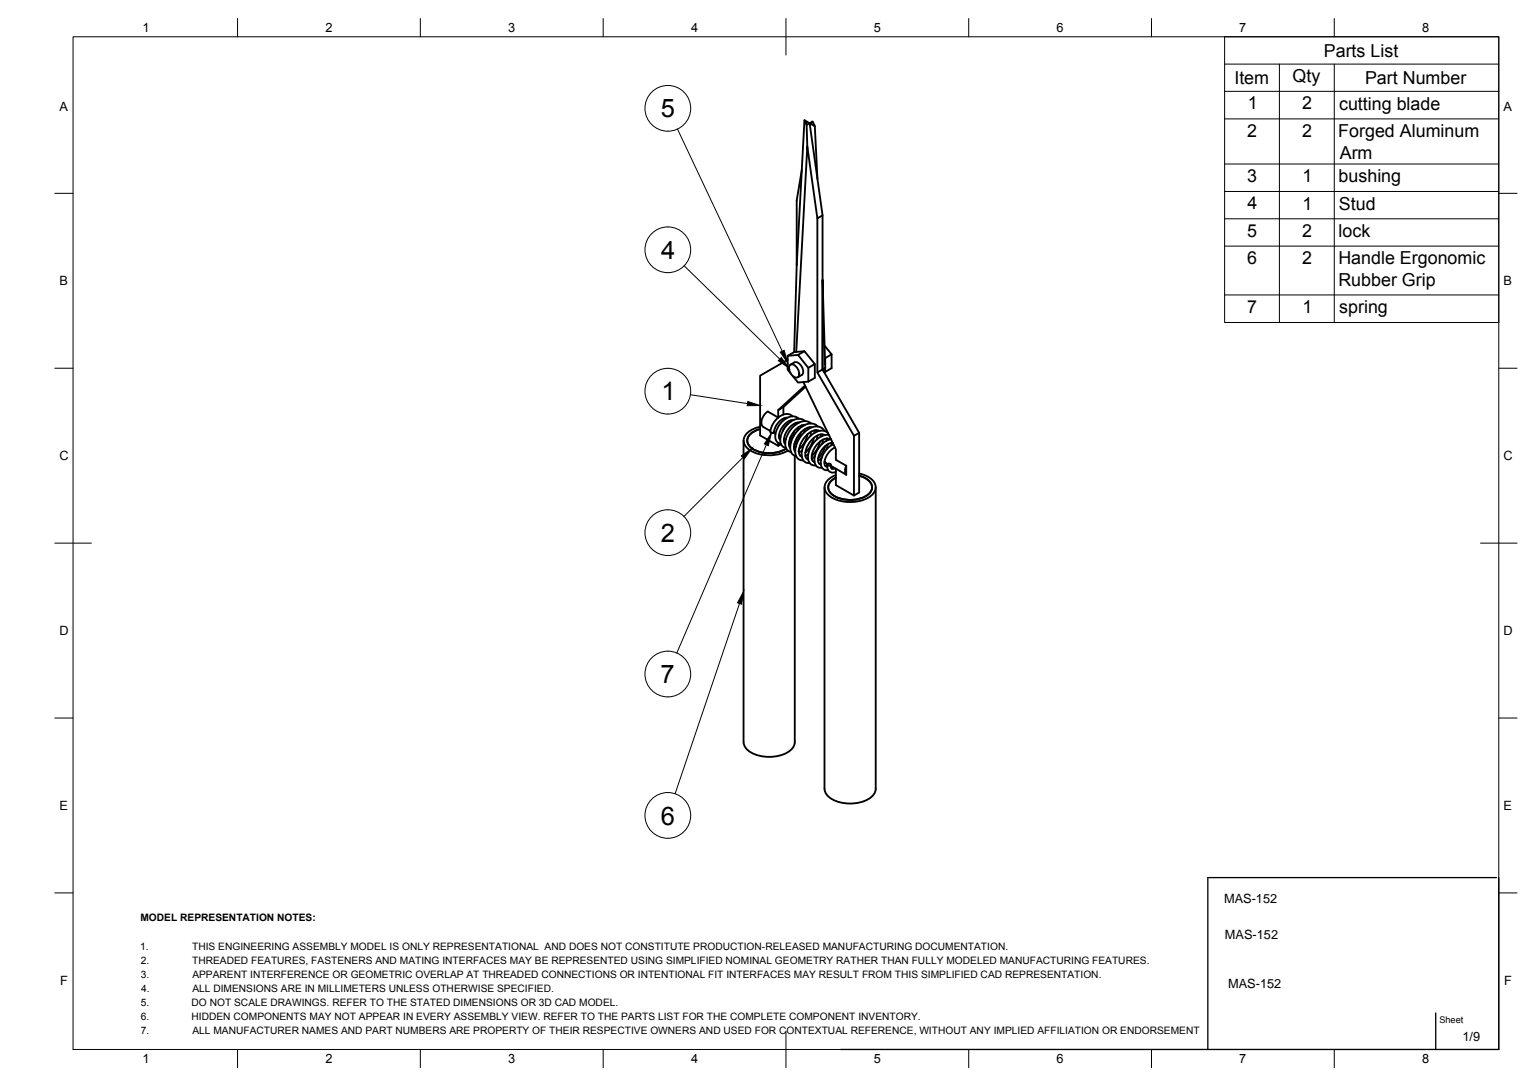
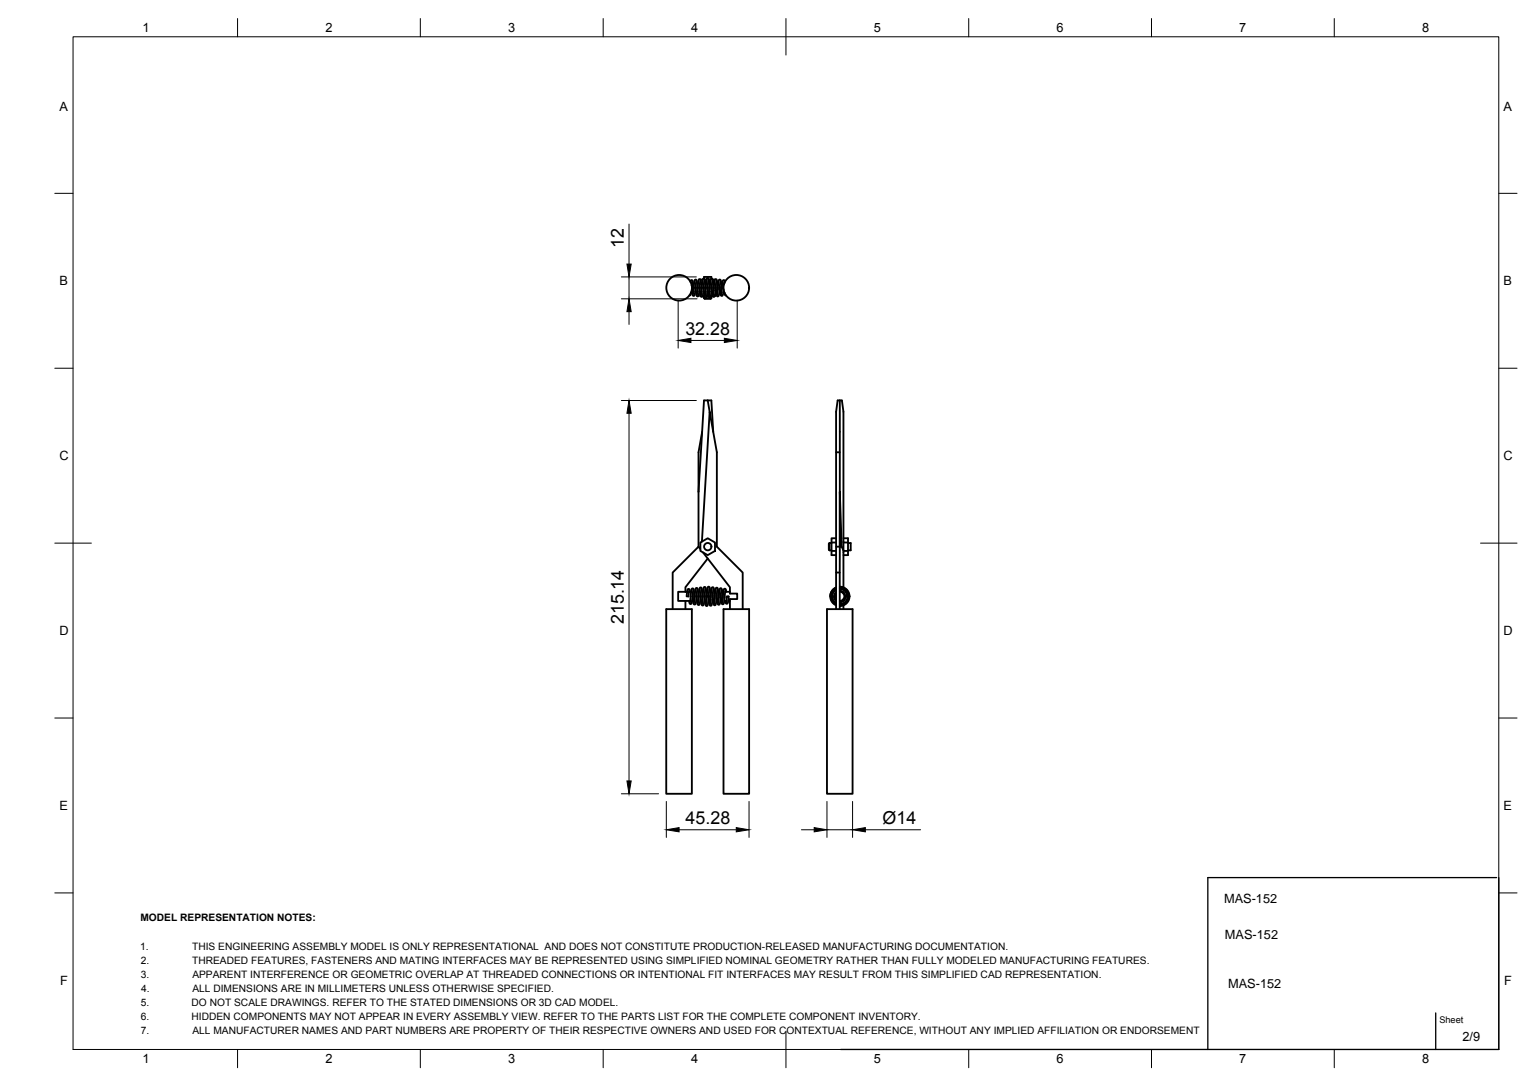
ISO-10303-21;
HEADER;
/* Generated by software containing ST-Developer
 * from STEP Tools, Inc. (www.steptools.com) 
 */

FILE_DESCRIPTION(
/* description */ ('STEP AP214'),
/* implementation_level */ '2;1');

FILE_NAME(
/* name */ 'MAS-152',
/* time_stamp */ '2026-11-04T19:18:53-08:00',
/* author */ (''),
/* organization */ (''),
/* preprocessor_version */ 'ST-DEVELOPER v20.2',
/* originating_system */ 'Autodesk Translation Framework v15.17.0.0',
/* authorisation */ '');

FILE_SCHEMA (('AUTOMOTIVE_DESIGN { 1 0 10303 214 3 1 1 }'));
ENDSEC;

DATA;
#10=MECHANICAL_DESIGN_GEOMETRIC_PRESENTATION_REPRESENTATION('',(#78,#79,
#80,#81,#82,#83,#84),#5942);
#11=ITEM_DEFINED_TRANSFORMATION($,$,#1040,#1100);
#12=ITEM_DEFINED_TRANSFORMATION($,$,#1067,#1101);
#13=ITEM_DEFINED_TRANSFORMATION($,$,#1011,#1102);
#14=ITEM_DEFINED_TRANSFORMATION($,$,#1020,#1103);
#15=ITEM_DEFINED_TRANSFORMATION($,$,#1088,#1104);
#16=ITEM_DEFINED_TRANSFORMATION($,$,#1078,#1105);
#17=ITEM_DEFINED_TRANSFORMATION($,$,#1029,#1106);
#18=ITEM_DEFINED_TRANSFORMATION($,$,#1040,#1107);
#19=ITEM_DEFINED_TRANSFORMATION($,$,#1067,#1108);
#20=ITEM_DEFINED_TRANSFORMATION($,$,#1078,#1109);
#21=ITEM_DEFINED_TRANSFORMATION($,$,#1088,#1110);
#22=(
REPRESENTATION_RELATIONSHIP($,$,#5978,#5974)
REPRESENTATION_RELATIONSHIP_WITH_TRANSFORMATION(#11)
SHAPE_REPRESENTATION_RELATIONSHIP()
);
#23=(
REPRESENTATION_RELATIONSHIP($,$,#5979,#5974)
REPRESENTATION_RELATIONSHIP_WITH_TRANSFORMATION(#12)
SHAPE_REPRESENTATION_RELATIONSHIP()
);
#24=(
REPRESENTATION_RELATIONSHIP($,$,#5975,#5974)
REPRESENTATION_RELATIONSHIP_WITH_TRANSFORMATION(#13)
SHAPE_REPRESENTATION_RELATIONSHIP()
);
#25=(
REPRESENTATION_RELATIONSHIP($,$,#5976,#5974)
REPRESENTATION_RELATIONSHIP_WITH_TRANSFORMATION(#14)
SHAPE_REPRESENTATION_RELATIONSHIP()
);
#26=(
REPRESENTATION_RELATIONSHIP($,$,#5981,#5974)
REPRESENTATION_RELATIONSHIP_WITH_TRANSFORMATION(#15)
SHAPE_REPRESENTATION_RELATIONSHIP()
);
#27=(
REPRESENTATION_RELATIONSHIP($,$,#5980,#5974)
REPRESENTATION_RELATIONSHIP_WITH_TRANSFORMATION(#16)
SHAPE_REPRESENTATION_RELATIONSHIP()
);
#28=(
REPRESENTATION_RELATIONSHIP($,$,#5977,#5974)
REPRESENTATION_RELATIONSHIP_WITH_TRANSFORMATION(#17)
SHAPE_REPRESENTATION_RELATIONSHIP()
);
#29=(
REPRESENTATION_RELATIONSHIP($,$,#5978,#5974)
REPRESENTATION_RELATIONSHIP_WITH_TRANSFORMATION(#18)
SHAPE_REPRESENTATION_RELATIONSHIP()
);
#30=(
REPRESENTATION_RELATIONSHIP($,$,#5979,#5974)
REPRESENTATION_RELATIONSHIP_WITH_TRANSFORMATION(#19)
SHAPE_REPRESENTATION_RELATIONSHIP()
);
#31=(
REPRESENTATION_RELATIONSHIP($,$,#5980,#5974)
REPRESENTATION_RELATIONSHIP_WITH_TRANSFORMATION(#20)
SHAPE_REPRESENTATION_RELATIONSHIP()
);
#32=(
REPRESENTATION_RELATIONSHIP($,$,#5981,#5974)
REPRESENTATION_RELATIONSHIP_WITH_TRANSFORMATION(#21)
SHAPE_REPRESENTATION_RELATIONSHIP()
);
#33=CONTEXT_DEPENDENT_SHAPE_REPRESENTATION(#22,#5963);
#34=CONTEXT_DEPENDENT_SHAPE_REPRESENTATION(#23,#5964);
#35=CONTEXT_DEPENDENT_SHAPE_REPRESENTATION(#24,#5965);
#36=CONTEXT_DEPENDENT_SHAPE_REPRESENTATION(#25,#5966);
#37=CONTEXT_DEPENDENT_SHAPE_REPRESENTATION(#26,#5967);
#38=CONTEXT_DEPENDENT_SHAPE_REPRESENTATION(#27,#5968);
#39=CONTEXT_DEPENDENT_SHAPE_REPRESENTATION(#28,#5969);
#40=CONTEXT_DEPENDENT_SHAPE_REPRESENTATION(#29,#5970);
#41=CONTEXT_DEPENDENT_SHAPE_REPRESENTATION(#30,#5971);
#42=CONTEXT_DEPENDENT_SHAPE_REPRESENTATION(#31,#5972);
#43=CONTEXT_DEPENDENT_SHAPE_REPRESENTATION(#32,#5973);
#44=NEXT_ASSEMBLY_USAGE_OCCURRENCE('Cutting Blade:1','Cutting Blade:1',
'Cutting Blade:1',#5983,#5987,'Cutting Blade:1');
#45=NEXT_ASSEMBLY_USAGE_OCCURRENCE('Forged Aluminum Arm:1',
'Forged Aluminum Arm:1','Forged Aluminum Arm:1',#5983,#5988,
'Forged Aluminum Arm:1');
#46=NEXT_ASSEMBLY_USAGE_OCCURRENCE('bushing:1','bushing:1','bushing:1',
#5983,#5984,'bushing:1');
#47=NEXT_ASSEMBLY_USAGE_OCCURRENCE('stud:1','stud:1','stud:1',#5983,#5985,
'stud:1');
#48=NEXT_ASSEMBLY_USAGE_OCCURRENCE('lock:1','lock:1','lock:1',#5983,#5990,
'lock:1');
#49=NEXT_ASSEMBLY_USAGE_OCCURRENCE('Handle Ergonomic Rubber Grip:1',
'Handle Ergonomic Rubber Grip:1','Handle Ergonomic Rubber Grip:1',#5983,
#5989,'Handle Ergonomic Rubber Grip:1');
#50=NEXT_ASSEMBLY_USAGE_OCCURRENCE('spring:1','spring:1','spring:1',#5983,
#5986,'spring:1');
#51=NEXT_ASSEMBLY_USAGE_OCCURRENCE('Cutting Blade:2','Cutting Blade:2',
'Cutting Blade:2',#5983,#5987,'Cutting Blade:2');
#52=NEXT_ASSEMBLY_USAGE_OCCURRENCE('Forged Aluminum Arm:2',
'Forged Aluminum Arm:2','Forged Aluminum Arm:2',#5983,#5988,
'Forged Aluminum Arm:2');
#53=NEXT_ASSEMBLY_USAGE_OCCURRENCE('Handle Ergonomic Rubber Grip:2',
'Handle Ergonomic Rubber Grip:2','Handle Ergonomic Rubber Grip:2',#5983,
#5989,'Handle Ergonomic Rubber Grip:2');
#54=NEXT_ASSEMBLY_USAGE_OCCURRENCE('lock:2','lock:2','lock:2',#5983,#5990,
'lock:2');
#55=B_SPLINE_CURVE_WITH_KNOTS('',3,(#2155,#2156,#2157,#2158,#2159,#2160,
#2161,#2162,#2163,#2164,#2165,#2166,#2167,#2168,#2169,#2170,#2171,#2172,
#2173,#2174,#2175,#2176,#2177,#2178,#2179,#2180,#2181,#2182,#2183,#2184,
#2185,#2186,#2187,#2188,#2189,#2190,#2191,#2192,#2193,#2194,#2195,#2196,
#2197,#2198,#2199,#2200,#2201,#2202,#2203,#2204,#2205,#2206,#2207,#2208,
#2209,#2210,#2211,#2212,#2213,#2214,#2215,#2216,#2217,#2218,#2219,#2220,
#2221,#2222,#2223,#2224,#2225,#2226,#2227,#2228,#2229,#2230,#2231,#2232,
#2233,#2234,#2235,#2236,#2237,#2238,#2239,#2240,#2241,#2242,#2243,#2244,
#2245,#2246,#2247,#2248,#2249,#2250,#2251,#2252,#2253,#2254,#2255,#2256,
#2257,#2258,#2259,#2260,#2261,#2262,#2263,#2264,#2265,#2266,#2267,#2268,
#2269,#2270,#2271,#2272,#2273,#2274,#2275,#2276,#2277,#2278,#2279,#2280,
#2281,#2282,#2283,#2284,#2285,#2286,#2287,#2288,#2289,#2290,#2291,#2292,
#2293,#2294,#2295,#2296,#2297,#2298,#2299,#2300,#2301,#2302,#2303,#2304,
#2305,#2306,#2307,#2308),.UNSPECIFIED.,.F.,.F.,(4,3,3,3,3,3,3,3,3,3,3,3,
3,3,3,3,3,3,3,3,3,3,3,3,3,3,3,3,3,3,3,3,3,3,3,3,3,3,3,3,3,3,3,3,3,3,3,3,
3,3,3,4),(8.16441129645516E-18,0.0155213821795324,0.0465641465385971,0.0776069108976618,
0.108649675256726,0.139692439615791,0.170735203974856,0.201777968333921,
0.232820732692985,0.26386349705205,0.294906261411162,0.325949025770274,
0.356991790129291,0.388034554488308,0.419077318847373,0.450120083206437,
0.46564146538597,0.481162847565502,0.496684229745034,0.512205611924566,
0.527726994104099,0.543248376283631,0.558769758463163,0.574291140642696,
0.589812522822228,0.605333905001761,0.620855287181293,0.636376669360825,
0.651898051540357,0.66741943371989,0.682940815899422,0.698462198078954,
0.713983580258487,0.729504962438019,0.745026344617551,0.760547726797084,
0.776069108976616,0.791590491156148,0.807111873335681,0.822633255515213,
0.838154637694745,0.853676019874278,0.86919740205381,0.884718784233342,
0.900240166412875,0.915761548592407,0.931282930771939,0.946804312951471,
0.973402156475736,0.986701078237868,0.993350539118934,0.993460673612188),
 .UNSPECIFIED.);
#56=B_SPLINE_CURVE_WITH_KNOTS('',3,(#2313,#2314,#2315,#2316,#2317,#2318,
#2319,#2320,#2321,#2322,#2323,#2324,#2325,#2326,#2327,#2328,#2329,#2330,
#2331,#2332,#2333,#2334,#2335,#2336,#2337,#2338,#2339,#2340,#2341,#2342,
#2343,#2344,#2345,#2346,#2347,#2348,#2349,#2350,#2351,#2352,#2353,#2354,
#2355,#2356,#2357,#2358,#2359,#2360,#2361,#2362,#2363,#2364,#2365,#2366,
#2367,#2368,#2369,#2370,#2371,#2372,#2373,#2374,#2375,#2376,#2377,#2378,
#2379,#2380,#2381,#2382,#2383,#2384,#2385,#2386,#2387,#2388,#2389,#2390,
#2391,#2392,#2393,#2394,#2395,#2396,#2397,#2398,#2399,#2400,#2401,#2402,
#2403,#2404,#2405,#2406,#2407,#2408,#2409,#2410,#2411,#2412,#2413,#2414,
#2415,#2416,#2417,#2418,#2419,#2420,#2421,#2422,#2423,#2424,#2425,#2426,
#2427,#2428,#2429,#2430,#2431,#2432,#2433,#2434,#2435,#2436,#2437,#2438,
#2439,#2440,#2441,#2442,#2443,#2444,#2445,#2446,#2447,#2448,#2449,#2450,
#2451,#2452,#2453,#2454,#2455,#2456,#2457,#2458,#2459,#2460,#2461,#2462,
#2463),.UNSPECIFIED.,.F.,.F.,(4,3,3,3,3,3,3,3,3,3,3,3,3,3,3,3,3,3,3,3,3,
3,3,3,3,3,3,3,3,3,3,3,3,3,3,3,3,3,3,3,3,3,3,3,3,3,3,3,3,3,4),(0.,0.0155213821795324,
0.0465641465385971,0.0776069108976618,0.108649675256726,0.139692439615791,
0.170735203974856,0.201777968333921,0.232820732692985,0.26386349705205,
0.294906261411162,0.325949025770274,0.356991790129291,0.388034554488308,
0.419077318847373,0.450120083206437,0.46564146538597,0.481162847565502,
0.496684229745034,0.512205611924566,0.527726994104099,0.543248376283631,
0.558769758463163,0.574291140642696,0.589812522822228,0.605333905001761,
0.620855287181293,0.636376669360825,0.651898051540357,0.66741943371989,
0.682940815899422,0.698462198078954,0.713983580258487,0.729504962438019,
0.745026344617551,0.760547726797084,0.776069108976616,0.791590491156148,
0.807111873335681,0.822633255515213,0.838154637694745,0.853676019874278,
0.86919740205381,0.884718784233342,0.900240166412875,0.915761548592407,
0.931282930771939,0.946804312951471,0.973402156475736,0.986701078237868,
0.993275477626297),.UNSPECIFIED.);
#57=B_SPLINE_CURVE_WITH_KNOTS('',3,(#3378,#3379,#3380,#3381,#3382,#3383,
#3384,#3385,#3386,#3387,#3388,#3389,#3390,#3391,#3392,#3393,#3394,#3395,
#3396,#3397,#3398,#3399,#3400,#3401,#3402,#3403,#3404,#3405,#3406,#3407,
#3408,#3409,#3410,#3411,#3412,#3413,#3414,#3415,#3416,#3417,#3418,#3419,
#3420,#3421,#3422,#3423,#3424,#3425,#3426,#3427,#3428,#3429,#3430,#3431,
#3432,#3433,#3434,#3435,#3436,#3437,#3438,#3439,#3440,#3441,#3442,#3443,
#3444,#3445,#3446,#3447,#3448,#3449,#3450,#3451,#3452,#3453,#3454,#3455,
#3456,#3457,#3458,#3459,#3460,#3461,#3462,#3463,#3464,#3465,#3466,#3467,
#3468,#3469,#3470,#3471,#3472,#3473,#3474,#3475,#3476,#3477,#3478,#3479,
#3480,#3481,#3482,#3483,#3484,#3485,#3486,#3487,#3488,#3489,#3490,#3491,
#3492,#3493,#3494,#3495,#3496,#3497,#3498,#3499,#3500,#3501,#3502,#3503,
#3504,#3505,#3506,#3507,#3508,#3509,#3510,#3511,#3512,#3513,#3514,#3515,
#3516,#3517,#3518,#3519,#3520,#3521,#3522,#3523,#3524,#3525,#3526,#3527,
#3528,#3529,#3530,#3531,#3532,#3533,#3534,#3535,#3536,#3537,#3538,#3539,
#3540,#3541,#3542,#3543,#3544,#3545,#3546,#3547,#3548,#3549,#3550,#3551,
#3552,#3553,#3554,#3555,#3556,#3557,#3558,#3559,#3560,#3561,#3562,#3563,
#3564,#3565,#3566,#3567,#3568,#3569,#3570),.UNSPECIFIED.,.F.,.F.,(4,3,3,
3,3,3,3,3,3,3,3,3,3,3,3,3,3,3,3,3,3,3,3,3,3,3,3,3,3,3,3,3,3,3,3,3,3,3,3,
3,3,3,3,3,3,3,3,3,3,3,3,3,3,3,3,3,3,3,3,3,3,3,3,3,4),(-3.92493609792139E-18,
0.015625,0.03125,0.046875,0.0625,0.078125,0.09375,0.109375,0.125,0.140625,
0.15625,0.171875,0.1875,0.203125,0.21875,0.234375,0.25,0.265625,0.28125,
0.296875,0.3125,0.328125,0.34375,0.359375,0.375,0.390625,0.40625,0.421875,
0.4375,0.453125,0.46875,0.484375,0.5,0.515625,0.53125,0.546875,0.5625,0.578125,
0.59375,0.609375,0.625,0.640625,0.65625,0.671875,0.6875,0.703125,0.71875,
0.734375,0.75,0.765625,0.78125,0.796875,0.8125,0.828125,0.84375,0.859375,
0.875,0.890625,0.90625,0.921875,0.9375,0.953125,0.96875,0.984375,1.),
 .UNSPECIFIED.);
#58=B_SPLINE_CURVE_WITH_KNOTS('',3,(#3572,#3573,#3574,#3575,#3576,#3577,
#3578,#3579,#3580,#3581,#3582,#3583,#3584,#3585,#3586,#3587,#3588,#3589,
#3590,#3591,#3592,#3593,#3594,#3595,#3596,#3597,#3598,#3599,#3600,#3601,
#3602,#3603,#3604,#3605,#3606,#3607,#3608,#3609,#3610,#3611,#3612,#3613,
#3614,#3615,#3616,#3617,#3618,#3619,#3620,#3621,#3622,#3623,#3624,#3625,
#3626,#3627,#3628,#3629,#3630,#3631,#3632,#3633,#3634,#3635,#3636,#3637,
#3638,#3639,#3640,#3641,#3642,#3643,#3644,#3645,#3646,#3647,#3648,#3649,
#3650,#3651,#3652,#3653,#3654,#3655,#3656,#3657,#3658,#3659,#3660,#3661,
#3662,#3663,#3664,#3665,#3666,#3667,#3668,#3669,#3670,#3671,#3672,#3673,
#3674,#3675,#3676,#3677,#3678,#3679,#3680,#3681,#3682,#3683,#3684,#3685,
#3686,#3687,#3688,#3689,#3690,#3691,#3692,#3693,#3694,#3695,#3696,#3697,
#3698,#3699,#3700,#3701,#3702,#3703,#3704,#3705,#3706,#3707,#3708,#3709,
#3710,#3711,#3712,#3713,#3714,#3715,#3716,#3717,#3718,#3719,#3720,#3721,
#3722,#3723,#3724,#3725,#3726,#3727,#3728,#3729,#3730,#3731,#3732,#3733,
#3734,#3735,#3736,#3737,#3738,#3739,#3740,#3741,#3742,#3743,#3744,#3745,
#3746,#3747,#3748,#3749,#3750,#3751,#3752,#3753,#3754,#3755,#3756,#3757,
#3758,#3759,#3760,#3761,#3762,#3763,#3764),.UNSPECIFIED.,.F.,.F.,(4,3,3,
3,3,3,3,3,3,3,3,3,3,3,3,3,3,3,3,3,3,3,3,3,3,3,3,3,3,3,3,3,3,3,3,3,3,3,3,
3,3,3,3,3,3,3,3,3,3,3,3,3,3,3,3,3,3,3,3,3,3,3,3,3,4),(0.,0.015625,0.03125,
0.046875,0.0625,0.078125,0.09375,0.109375,0.125,0.140625,0.15625,0.171875,
0.1875,0.203125,0.21875,0.234375,0.25,0.265625,0.28125,0.296875,0.3125,
0.328125,0.34375,0.359375,0.375,0.390625,0.40625,0.421875,0.4375,0.453125,
0.46875,0.484375,0.5,0.515625,0.53125,0.546875,0.5625,0.578125,0.59375,
0.609375,0.625,0.640625,0.65625,0.671875,0.6875,0.703125,0.71875,0.734375,
0.75,0.765625,0.78125,0.796875,0.8125,0.828125,0.84375,0.859375,0.875,0.890625,
0.90625,0.921875,0.9375,0.953125,0.96875,0.984375,1.),.UNSPECIFIED.);
#59=(
BOUNDED_SURFACE()
B_SPLINE_SURFACE(3,3,((#1423,#1424,#1425,#1426,#1427,#1428,#1429,#1430,
#1431,#1432,#1433,#1434,#1435,#1436,#1437,#1438,#1439,#1440,#1441,#1442,
#1443,#1444,#1445,#1446,#1447,#1448,#1449,#1450,#1451,#1452,#1453,#1454,
#1455,#1456,#1457,#1458,#1459,#1460,#1461,#1462,#1463,#1464,#1465,#1466,
#1467,#1468,#1469,#1470,#1471,#1472,#1473,#1474,#1475,#1476,#1477,#1478,
#1479,#1480,#1481,#1482,#1483,#1484,#1485,#1486,#1487,#1488,#1489,#1490,
#1491,#1492,#1493,#1494,#1495,#1496,#1497,#1498,#1499,#1500,#1501,#1502,
#1503,#1504,#1505,#1506,#1507,#1508,#1509,#1510,#1511,#1512,#1513,#1514,
#1515,#1516,#1517,#1518,#1519,#1520,#1521,#1522,#1523,#1524,#1525,#1526),
(#1527,#1528,#1529,#1530,#1531,#1532,#1533,#1534,#1535,#1536,#1537,#1538,
#1539,#1540,#1541,#1542,#1543,#1544,#1545,#1546,#1547,#1548,#1549,#1550,
#1551,#1552,#1553,#1554,#1555,#1556,#1557,#1558,#1559,#1560,#1561,#1562,
#1563,#1564,#1565,#1566,#1567,#1568,#1569,#1570,#1571,#1572,#1573,#1574,
#1575,#1576,#1577,#1578,#1579,#1580,#1581,#1582,#1583,#1584,#1585,#1586,
#1587,#1588,#1589,#1590,#1591,#1592,#1593,#1594,#1595,#1596,#1597,#1598,
#1599,#1600,#1601,#1602,#1603,#1604,#1605,#1606,#1607,#1608,#1609,#1610,
#1611,#1612,#1613,#1614,#1615,#1616,#1617,#1618,#1619,#1620,#1621,#1622,
#1623,#1624,#1625,#1626,#1627,#1628,#1629,#1630),(#1631,#1632,#1633,#1634,
#1635,#1636,#1637,#1638,#1639,#1640,#1641,#1642,#1643,#1644,#1645,#1646,
#1647,#1648,#1649,#1650,#1651,#1652,#1653,#1654,#1655,#1656,#1657,#1658,
#1659,#1660,#1661,#1662,#1663,#1664,#1665,#1666,#1667,#1668,#1669,#1670,
#1671,#1672,#1673,#1674,#1675,#1676,#1677,#1678,#1679,#1680,#1681,#1682,
#1683,#1684,#1685,#1686,#1687,#1688,#1689,#1690,#1691,#1692,#1693,#1694,
#1695,#1696,#1697,#1698,#1699,#1700,#1701,#1702,#1703,#1704,#1705,#1706,
#1707,#1708,#1709,#1710,#1711,#1712,#1713,#1714,#1715,#1716,#1717,#1718,
#1719,#1720,#1721,#1722,#1723,#1724,#1725,#1726,#1727,#1728,#1729,#1730,
#1731,#1732,#1733,#1734),(#1735,#1736,#1737,#1738,#1739,#1740,#1741,#1742,
#1743,#1744,#1745,#1746,#1747,#1748,#1749,#1750,#1751,#1752,#1753,#1754,
#1755,#1756,#1757,#1758,#1759,#1760,#1761,#1762,#1763,#1764,#1765,#1766,
#1767,#1768,#1769,#1770,#1771,#1772,#1773,#1774,#1775,#1776,#1777,#1778,
#1779,#1780,#1781,#1782,#1783,#1784,#1785,#1786,#1787,#1788,#1789,#1790,
#1791,#1792,#1793,#1794,#1795,#1796,#1797,#1798,#1799,#1800,#1801,#1802,
#1803,#1804,#1805,#1806,#1807,#1808,#1809,#1810,#1811,#1812,#1813,#1814,
#1815,#1816,#1817,#1818,#1819,#1820,#1821,#1822,#1823,#1824,#1825,#1826,
#1827,#1828,#1829,#1830,#1831,#1832,#1833,#1834,#1835,#1836,#1837,#1838),
(#1839,#1840,#1841,#1842,#1843,#1844,#1845,#1846,#1847,#1848,#1849,#1850,
#1851,#1852,#1853,#1854,#1855,#1856,#1857,#1858,#1859,#1860,#1861,#1862,
#1863,#1864,#1865,#1866,#1867,#1868,#1869,#1870,#1871,#1872,#1873,#1874,
#1875,#1876,#1877,#1878,#1879,#1880,#1881,#1882,#1883,#1884,#1885,#1886,
#1887,#1888,#1889,#1890,#1891,#1892,#1893,#1894,#1895,#1896,#1897,#1898,
#1899,#1900,#1901,#1902,#1903,#1904,#1905,#1906,#1907,#1908,#1909,#1910,
#1911,#1912,#1913,#1914,#1915,#1916,#1917,#1918,#1919,#1920,#1921,#1922,
#1923,#1924,#1925,#1926,#1927,#1928,#1929,#1930,#1931,#1932,#1933,#1934,
#1935,#1936,#1937,#1938,#1939,#1940,#1941,#1942),(#1943,#1944,#1945,#1946,
#1947,#1948,#1949,#1950,#1951,#1952,#1953,#1954,#1955,#1956,#1957,#1958,
#1959,#1960,#1961,#1962,#1963,#1964,#1965,#1966,#1967,#1968,#1969,#1970,
#1971,#1972,#1973,#1974,#1975,#1976,#1977,#1978,#1979,#1980,#1981,#1982,
#1983,#1984,#1985,#1986,#1987,#1988,#1989,#1990,#1991,#1992,#1993,#1994,
#1995,#1996,#1997,#1998,#1999,#2000,#2001,#2002,#2003,#2004,#2005,#2006,
#2007,#2008,#2009,#2010,#2011,#2012,#2013,#2014,#2015,#2016,#2017,#2018,
#2019,#2020,#2021,#2022,#2023,#2024,#2025,#2026,#2027,#2028,#2029,#2030,
#2031,#2032,#2033,#2034,#2035,#2036,#2037,#2038,#2039,#2040,#2041,#2042,
#2043,#2044,#2045,#2046),(#2047,#2048,#2049,#2050,#2051,#2052,#2053,#2054,
#2055,#2056,#2057,#2058,#2059,#2060,#2061,#2062,#2063,#2064,#2065,#2066,
#2067,#2068,#2069,#2070,#2071,#2072,#2073,#2074,#2075,#2076,#2077,#2078,
#2079,#2080,#2081,#2082,#2083,#2084,#2085,#2086,#2087,#2088,#2089,#2090,
#2091,#2092,#2093,#2094,#2095,#2096,#2097,#2098,#2099,#2100,#2101,#2102,
#2103,#2104,#2105,#2106,#2107,#2108,#2109,#2110,#2111,#2112,#2113,#2114,
#2115,#2116,#2117,#2118,#2119,#2120,#2121,#2122,#2123,#2124,#2125,#2126,
#2127,#2128,#2129,#2130,#2131,#2132,#2133,#2134,#2135,#2136,#2137,#2138,
#2139,#2140,#2141,#2142,#2143,#2144,#2145,#2146,#2147,#2148,#2149,#2150)),
 .UNSPECIFIED.,.T.,.F.,.F.)
B_SPLINE_SURFACE_WITH_KNOTS((4,3,4),(4,2,2,2,2,2,2,2,2,2,2,2,2,2,2,2,2,
2,2,2,2,2,2,2,2,2,2,2,2,2,2,2,2,2,2,2,2,2,2,2,2,2,2,2,2,2,2,2,2,2,2,4),
(0.,0.5,1.),(0.,0.0155213821795324,0.0465641465385971,0.0776069108976618,
0.108649675256726,0.139692439615791,0.170735203974856,0.201777968333921,
0.232820732692985,0.26386349705205,0.294906261411162,0.325949025770274,
0.356991790129291,0.388034554488308,0.419077318847373,0.450120083206437,
0.46564146538597,0.481162847565502,0.496684229745034,0.512205611924566,
0.527726994104099,0.543248376283631,0.558769758463163,0.574291140642696,
0.589812522822228,0.605333905001761,0.620855287181293,0.636376669360825,
0.651898051540357,0.66741943371989,0.682940815899422,0.698462198078954,
0.713983580258487,0.729504962438019,0.745026344617551,0.760547726797084,
0.776069108976616,0.791590491156148,0.807111873335681,0.822633255515213,
0.838154637694745,0.853676019874278,0.86919740205381,0.884718784233342,
0.900240166412875,0.915761548592407,0.931282930771939,0.946804312951471,
0.973402156475736,0.986701078237868,0.993350539118934,1.),.UNSPECIFIED.)
GEOMETRIC_REPRESENTATION_ITEM()
RATIONAL_B_SPLINE_SURFACE(((1.,1.,1.,1.,1.,1.,1.,1.,1.,1.,1.,1.,1.,1.,1.,
1.,1.,1.,1.,1.,1.,1.,1.,1.,1.,1.,1.,1.,1.,1.,1.,1.,1.,1.,1.,1.,1.,1.,1.,
1.,1.,1.,1.,1.,1.,1.,1.,1.,1.,1.,1.,1.,1.,1.,1.,1.,1.,1.,1.,1.,1.,1.,1.,
1.,1.,1.,1.,1.,1.,1.,1.,1.,1.,1.,1.,1.,1.,1.,1.,1.,1.,1.,1.,1.,1.,1.,1.,
1.,1.,1.,1.,1.,1.,1.,1.,1.,1.,1.,1.,1.,1.,1.,1.,1.),(0.333333333333333,
0.333333333333333,0.333333333333333,0.333333333333333,0.333333333333333,
0.333333333333333,0.333333333333333,0.333333333333333,0.333333333333333,
0.333333333333333,0.333333333333333,0.333333333333333,0.333333333333333,
0.333333333333333,0.333333333333333,0.333333333333333,0.333333333333333,
0.333333333333333,0.333333333333333,0.333333333333333,0.333333333333333,
0.333333333333333,0.333333333333333,0.333333333333333,0.333333333333333,
0.333333333333333,0.333333333333333,0.333333333333333,0.333333333333333,
0.333333333333333,0.333333333333333,0.333333333333333,0.333333333333333,
0.333333333333333,0.333333333333333,0.333333333333333,0.333333333333333,
0.333333333333333,0.333333333333333,0.333333333333333,0.333333333333333,
0.333333333333333,0.333333333333333,0.333333333333333,0.333333333333333,
0.333333333333333,0.333333333333333,0.333333333333333,0.333333333333333,
0.333333333333333,0.333333333333333,0.333333333333333,0.333333333333333,
0.333333333333333,0.333333333333333,0.333333333333333,0.333333333333333,
0.333333333333333,0.333333333333333,0.333333333333333,0.333333333333333,
0.333333333333333,0.333333333333333,0.333333333333333,0.333333333333333,
0.333333333333333,0.333333333333333,0.333333333333333,0.333333333333333,
0.333333333333333,0.333333333333333,0.333333333333333,0.333333333333333,
0.333333333333333,0.333333333333333,0.333333333333333,0.333333333333333,
0.333333333333333,0.333333333333333,0.333333333333333,0.333333333333333,
0.333333333333333,0.333333333333333,0.333333333333333,0.333333333333333,
0.333333333333333,0.333333333333333,0.333333333333333,0.333333333333333,
0.333333333333333,0.333333333333333,0.333333333333333,0.333333333333333,
0.333333333333333,0.333333333333333,0.333333333333333,0.333333333333333,
0.333333333333333,0.333333333333333,0.333333333333333,0.333333333333333,
0.333333333333333,0.333333333333333,0.333333333333333),(0.333333333333333,
0.333333333333333,0.333333333333333,0.333333333333333,0.333333333333333,
0.333333333333333,0.333333333333333,0.333333333333333,0.333333333333333,
0.333333333333333,0.333333333333333,0.333333333333333,0.333333333333333,
0.333333333333333,0.333333333333333,0.333333333333333,0.333333333333333,
0.333333333333333,0.333333333333333,0.333333333333333,0.333333333333333,
0.333333333333333,0.333333333333333,0.333333333333333,0.333333333333333,
0.333333333333333,0.333333333333333,0.333333333333333,0.333333333333333,
0.333333333333333,0.333333333333333,0.333333333333333,0.333333333333333,
0.333333333333333,0.333333333333333,0.333333333333333,0.333333333333333,
0.333333333333333,0.333333333333333,0.333333333333333,0.333333333333333,
0.333333333333333,0.333333333333333,0.333333333333333,0.333333333333333,
0.333333333333333,0.333333333333333,0.333333333333333,0.333333333333333,
0.333333333333333,0.333333333333333,0.333333333333333,0.333333333333333,
0.333333333333333,0.333333333333333,0.333333333333333,0.333333333333333,
0.333333333333333,0.333333333333333,0.333333333333333,0.333333333333333,
0.333333333333333,0.333333333333333,0.333333333333333,0.333333333333333,
0.333333333333333,0.333333333333333,0.333333333333333,0.333333333333333,
0.333333333333333,0.333333333333333,0.333333333333333,0.333333333333333,
0.333333333333333,0.333333333333333,0.333333333333333,0.333333333333333,
0.333333333333333,0.333333333333333,0.333333333333333,0.333333333333333,
0.333333333333333,0.333333333333333,0.333333333333333,0.333333333333333,
0.333333333333333,0.333333333333333,0.333333333333333,0.333333333333333,
0.333333333333333,0.333333333333333,0.333333333333333,0.333333333333333,
0.333333333333333,0.333333333333333,0.333333333333333,0.333333333333333,
0.333333333333333,0.333333333333333,0.333333333333333,0.333333333333333,
0.333333333333333,0.333333333333333,0.333333333333333),(1.,1.,1.,1.,1.,
1.,1.,1.,1.,1.,1.,1.,1.,1.,1.,1.,1.,1.,1.,1.,1.,1.,1.,1.,1.,1.,1.,1.,1.,
1.,1.,1.,1.,1.,1.,1.,1.,1.,1.,1.,1.,1.,1.,1.,1.,1.,1.,1.,1.,1.,1.,1.,1.,
1.,1.,1.,1.,1.,1.,1.,1.,1.,1.,1.,1.,1.,1.,1.,1.,1.,1.,1.,1.,1.,1.,1.,1.,
1.,1.,1.,1.,1.,1.,1.,1.,1.,1.,1.,1.,1.,1.,1.,1.,1.,1.,1.,1.,1.,1.,1.,1.,
1.,1.,1.),(0.333333333333333,0.333333333333333,0.333333333333333,0.333333333333333,
0.333333333333333,0.333333333333333,0.333333333333333,0.333333333333333,
0.333333333333333,0.333333333333333,0.333333333333333,0.333333333333333,
0.333333333333333,0.333333333333333,0.333333333333333,0.333333333333333,
0.333333333333333,0.333333333333333,0.333333333333333,0.333333333333333,
0.333333333333333,0.333333333333333,0.333333333333333,0.333333333333333,
0.333333333333333,0.333333333333333,0.333333333333333,0.333333333333333,
0.333333333333333,0.333333333333333,0.333333333333333,0.333333333333333,
0.333333333333333,0.333333333333333,0.333333333333333,0.333333333333333,
0.333333333333333,0.333333333333333,0.333333333333333,0.333333333333333,
0.333333333333333,0.333333333333333,0.333333333333333,0.333333333333333,
0.333333333333333,0.333333333333333,0.333333333333333,0.333333333333333,
0.333333333333333,0.333333333333333,0.333333333333333,0.333333333333333,
0.333333333333333,0.333333333333333,0.333333333333333,0.333333333333333,
0.333333333333333,0.333333333333333,0.333333333333333,0.333333333333333,
0.333333333333333,0.333333333333333,0.333333333333333,0.333333333333333,
0.333333333333333,0.333333333333333,0.333333333333333,0.333333333333333,
0.333333333333333,0.333333333333333,0.333333333333333,0.333333333333333,
0.333333333333333,0.333333333333333,0.333333333333333,0.333333333333333,
0.333333333333333,0.333333333333333,0.333333333333333,0.333333333333333,
0.333333333333333,0.333333333333333,0.333333333333333,0.333333333333333,
0.333333333333333,0.333333333333333,0.333333333333333,0.333333333333333,
0.333333333333333,0.333333333333333,0.333333333333333,0.333333333333333,
0.333333333333333,0.333333333333333,0.333333333333333,0.333333333333333,
0.333333333333333,0.333333333333333,0.333333333333333,0.333333333333333,
0.333333333333333,0.333333333333333,0.333333333333333,0.333333333333333),
(0.333333333333333,0.333333333333333,0.333333333333333,0.333333333333333,
0.333333333333333,0.333333333333333,0.333333333333333,0.333333333333333,
0.333333333333333,0.333333333333333,0.333333333333333,0.333333333333333,
0.333333333333333,0.333333333333333,0.333333333333333,0.333333333333333,
0.333333333333333,0.333333333333333,0.333333333333333,0.333333333333333,
0.333333333333333,0.333333333333333,0.333333333333333,0.333333333333333,
0.333333333333333,0.333333333333333,0.333333333333333,0.333333333333333,
0.333333333333333,0.333333333333333,0.333333333333333,0.333333333333333,
0.333333333333333,0.333333333333333,0.333333333333333,0.333333333333333,
0.333333333333333,0.333333333333333,0.333333333333333,0.333333333333333,
0.333333333333333,0.333333333333333,0.333333333333333,0.333333333333333,
0.333333333333333,0.333333333333333,0.333333333333333,0.333333333333333,
0.333333333333333,0.333333333333333,0.333333333333333,0.333333333333333,
0.333333333333333,0.333333333333333,0.333333333333333,0.333333333333333,
0.333333333333333,0.333333333333333,0.333333333333333,0.333333333333333,
0.333333333333333,0.333333333333333,0.333333333333333,0.333333333333333,
0.333333333333333,0.333333333333333,0.333333333333333,0.333333333333333,
0.333333333333333,0.333333333333333,0.333333333333333,0.333333333333333,
0.333333333333333,0.333333333333333,0.333333333333333,0.333333333333333,
0.333333333333333,0.333333333333333,0.333333333333333,0.333333333333333,
0.333333333333333,0.333333333333333,0.333333333333333,0.333333333333333,
0.333333333333333,0.333333333333333,0.333333333333333,0.333333333333333,
0.333333333333333,0.333333333333333,0.333333333333333,0.333333333333333,
0.333333333333333,0.333333333333333,0.333333333333333,0.333333333333333,
0.333333333333333,0.333333333333333,0.333333333333333,0.333333333333333,
0.333333333333333,0.333333333333333,0.333333333333333,0.333333333333333),
(1.,1.,1.,1.,1.,1.,1.,1.,1.,1.,1.,1.,1.,1.,1.,1.,1.,1.,1.,1.,1.,1.,1.,1.,
1.,1.,1.,1.,1.,1.,1.,1.,1.,1.,1.,1.,1.,1.,1.,1.,1.,1.,1.,1.,1.,1.,1.,1.,
1.,1.,1.,1.,1.,1.,1.,1.,1.,1.,1.,1.,1.,1.,1.,1.,1.,1.,1.,1.,1.,1.,1.,1.,
1.,1.,1.,1.,1.,1.,1.,1.,1.,1.,1.,1.,1.,1.,1.,1.,1.,1.,1.,1.,1.,1.,1.,1.,
1.,1.,1.,1.,1.,1.,1.,1.)))
REPRESENTATION_ITEM('')
SURFACE()
);
#60=(
BOUNDED_SURFACE()
B_SPLINE_SURFACE(3,3,((#2464,#2465,#2466,#2467,#2468,#2469,#2470,#2471,
#2472,#2473,#2474,#2475,#2476,#2477,#2478,#2479,#2480,#2481,#2482,#2483,
#2484,#2485,#2486,#2487,#2488,#2489,#2490,#2491,#2492,#2493,#2494,#2495,
#2496,#2497,#2498,#2499,#2500,#2501,#2502,#2503,#2504,#2505,#2506,#2507,
#2508,#2509,#2510,#2511,#2512,#2513,#2514,#2515,#2516,#2517,#2518,#2519,
#2520,#2521,#2522,#2523,#2524,#2525,#2526,#2527,#2528,#2529,#2530,#2531,
#2532,#2533,#2534,#2535,#2536,#2537,#2538,#2539,#2540,#2541,#2542,#2543,
#2544,#2545,#2546,#2547,#2548,#2549,#2550,#2551,#2552,#2553,#2554,#2555,
#2556,#2557,#2558,#2559,#2560,#2561,#2562,#2563,#2564,#2565,#2566,#2567,
#2568,#2569,#2570,#2571,#2572,#2573,#2574,#2575,#2576,#2577,#2578,#2579,
#2580,#2581,#2582,#2583,#2584,#2585,#2586,#2587,#2588,#2589,#2590,#2591,
#2592,#2593),(#2594,#2595,#2596,#2597,#2598,#2599,#2600,#2601,#2602,#2603,
#2604,#2605,#2606,#2607,#2608,#2609,#2610,#2611,#2612,#2613,#2614,#2615,
#2616,#2617,#2618,#2619,#2620,#2621,#2622,#2623,#2624,#2625,#2626,#2627,
#2628,#2629,#2630,#2631,#2632,#2633,#2634,#2635,#2636,#2637,#2638,#2639,
#2640,#2641,#2642,#2643,#2644,#2645,#2646,#2647,#2648,#2649,#2650,#2651,
#2652,#2653,#2654,#2655,#2656,#2657,#2658,#2659,#2660,#2661,#2662,#2663,
#2664,#2665,#2666,#2667,#2668,#2669,#2670,#2671,#2672,#2673,#2674,#2675,
#2676,#2677,#2678,#2679,#2680,#2681,#2682,#2683,#2684,#2685,#2686,#2687,
#2688,#2689,#2690,#2691,#2692,#2693,#2694,#2695,#2696,#2697,#2698,#2699,
#2700,#2701,#2702,#2703,#2704,#2705,#2706,#2707,#2708,#2709,#2710,#2711,
#2712,#2713,#2714,#2715,#2716,#2717,#2718,#2719,#2720,#2721,#2722,#2723),
(#2724,#2725,#2726,#2727,#2728,#2729,#2730,#2731,#2732,#2733,#2734,#2735,
#2736,#2737,#2738,#2739,#2740,#2741,#2742,#2743,#2744,#2745,#2746,#2747,
#2748,#2749,#2750,#2751,#2752,#2753,#2754,#2755,#2756,#2757,#2758,#2759,
#2760,#2761,#2762,#2763,#2764,#2765,#2766,#2767,#2768,#2769,#2770,#2771,
#2772,#2773,#2774,#2775,#2776,#2777,#2778,#2779,#2780,#2781,#2782,#2783,
#2784,#2785,#2786,#2787,#2788,#2789,#2790,#2791,#2792,#2793,#2794,#2795,
#2796,#2797,#2798,#2799,#2800,#2801,#2802,#2803,#2804,#2805,#2806,#2807,
#2808,#2809,#2810,#2811,#2812,#2813,#2814,#2815,#2816,#2817,#2818,#2819,
#2820,#2821,#2822,#2823,#2824,#2825,#2826,#2827,#2828,#2829,#2830,#2831,
#2832,#2833,#2834,#2835,#2836,#2837,#2838,#2839,#2840,#2841,#2842,#2843,
#2844,#2845,#2846,#2847,#2848,#2849,#2850,#2851,#2852,#2853),(#2854,#2855,
#2856,#2857,#2858,#2859,#2860,#2861,#2862,#2863,#2864,#2865,#2866,#2867,
#2868,#2869,#2870,#2871,#2872,#2873,#2874,#2875,#2876,#2877,#2878,#2879,
#2880,#2881,#2882,#2883,#2884,#2885,#2886,#2887,#2888,#2889,#2890,#2891,
#2892,#2893,#2894,#2895,#2896,#2897,#2898,#2899,#2900,#2901,#2902,#2903,
#2904,#2905,#2906,#2907,#2908,#2909,#2910,#2911,#2912,#2913,#2914,#2915,
#2916,#2917,#2918,#2919,#2920,#2921,#2922,#2923,#2924,#2925,#2926,#2927,
#2928,#2929,#2930,#2931,#2932,#2933,#2934,#2935,#2936,#2937,#2938,#2939,
#2940,#2941,#2942,#2943,#2944,#2945,#2946,#2947,#2948,#2949,#2950,#2951,
#2952,#2953,#2954,#2955,#2956,#2957,#2958,#2959,#2960,#2961,#2962,#2963,
#2964,#2965,#2966,#2967,#2968,#2969,#2970,#2971,#2972,#2973,#2974,#2975,
#2976,#2977,#2978,#2979,#2980,#2981,#2982,#2983),(#2984,#2985,#2986,#2987,
#2988,#2989,#2990,#2991,#2992,#2993,#2994,#2995,#2996,#2997,#2998,#2999,
#3000,#3001,#3002,#3003,#3004,#3005,#3006,#3007,#3008,#3009,#3010,#3011,
#3012,#3013,#3014,#3015,#3016,#3017,#3018,#3019,#3020,#3021,#3022,#3023,
#3024,#3025,#3026,#3027,#3028,#3029,#3030,#3031,#3032,#3033,#3034,#3035,
#3036,#3037,#3038,#3039,#3040,#3041,#3042,#3043,#3044,#3045,#3046,#3047,
#3048,#3049,#3050,#3051,#3052,#3053,#3054,#3055,#3056,#3057,#3058,#3059,
#3060,#3061,#3062,#3063,#3064,#3065,#3066,#3067,#3068,#3069,#3070,#3071,
#3072,#3073,#3074,#3075,#3076,#3077,#3078,#3079,#3080,#3081,#3082,#3083,
#3084,#3085,#3086,#3087,#3088,#3089,#3090,#3091,#3092,#3093,#3094,#3095,
#3096,#3097,#3098,#3099,#3100,#3101,#3102,#3103,#3104,#3105,#3106,#3107,
#3108,#3109,#3110,#3111,#3112,#3113),(#3114,#3115,#3116,#3117,#3118,#3119,
#3120,#3121,#3122,#3123,#3124,#3125,#3126,#3127,#3128,#3129,#3130,#3131,
#3132,#3133,#3134,#3135,#3136,#3137,#3138,#3139,#3140,#3141,#3142,#3143,
#3144,#3145,#3146,#3147,#3148,#3149,#3150,#3151,#3152,#3153,#3154,#3155,
#3156,#3157,#3158,#3159,#3160,#3161,#3162,#3163,#3164,#3165,#3166,#3167,
#3168,#3169,#3170,#3171,#3172,#3173,#3174,#3175,#3176,#3177,#3178,#3179,
#3180,#3181,#3182,#3183,#3184,#3185,#3186,#3187,#3188,#3189,#3190,#3191,
#3192,#3193,#3194,#3195,#3196,#3197,#3198,#3199,#3200,#3201,#3202,#3203,
#3204,#3205,#3206,#3207,#3208,#3209,#3210,#3211,#3212,#3213,#3214,#3215,
#3216,#3217,#3218,#3219,#3220,#3221,#3222,#3223,#3224,#3225,#3226,#3227,
#3228,#3229,#3230,#3231,#3232,#3233,#3234,#3235,#3236,#3237,#3238,#3239,
#3240,#3241,#3242,#3243),(#3244,#3245,#3246,#3247,#3248,#3249,#3250,#3251,
#3252,#3253,#3254,#3255,#3256,#3257,#3258,#3259,#3260,#3261,#3262,#3263,
#3264,#3265,#3266,#3267,#3268,#3269,#3270,#3271,#3272,#3273,#3274,#3275,
#3276,#3277,#3278,#3279,#3280,#3281,#3282,#3283,#3284,#3285,#3286,#3287,
#3288,#3289,#3290,#3291,#3292,#3293,#3294,#3295,#3296,#3297,#3298,#3299,
#3300,#3301,#3302,#3303,#3304,#3305,#3306,#3307,#3308,#3309,#3310,#3311,
#3312,#3313,#3314,#3315,#3316,#3317,#3318,#3319,#3320,#3321,#3322,#3323,
#3324,#3325,#3326,#3327,#3328,#3329,#3330,#3331,#3332,#3333,#3334,#3335,
#3336,#3337,#3338,#3339,#3340,#3341,#3342,#3343,#3344,#3345,#3346,#3347,
#3348,#3349,#3350,#3351,#3352,#3353,#3354,#3355,#3356,#3357,#3358,#3359,
#3360,#3361,#3362,#3363,#3364,#3365,#3366,#3367,#3368,#3369,#3370,#3371,
#3372,#3373)),.UNSPECIFIED.,.T.,.F.,.F.)
B_SPLINE_SURFACE_WITH_KNOTS((4,3,4),(4,2,2,2,2,2,2,2,2,2,2,2,2,2,2,2,2,
2,2,2,2,2,2,2,2,2,2,2,2,2,2,2,2,2,2,2,2,2,2,2,2,2,2,2,2,2,2,2,2,2,2,2,2,
2,2,2,2,2,2,2,2,2,2,2,4),(-6.51498550334715E-7,0.5,0.99999934850145),(0.,
0.015625,0.03125,0.046875,0.0625,0.078125,0.09375,0.109375,0.125,0.140625,
0.15625,0.171875,0.1875,0.203125,0.21875,0.234375,0.25,0.265625,0.28125,
0.296875,0.3125,0.328125,0.34375,0.359375,0.375,0.390625,0.40625,0.421875,
0.4375,0.453125,0.46875,0.484375,0.5,0.515625,0.53125,0.546875,0.5625,0.578125,
0.59375,0.609375,0.625,0.640625,0.65625,0.671875,0.6875,0.703125,0.71875,
0.734375,0.75,0.765625,0.78125,0.796875,0.8125,0.828125,0.84375,0.859375,
0.875,0.890625,0.90625,0.921875,0.9375,0.953125,0.96875,0.984375,1.),
 .UNSPECIFIED.)
GEOMETRIC_REPRESENTATION_ITEM()
RATIONAL_B_SPLINE_SURFACE(((0.999997394009194,0.999997394009194,0.999997394009194,
0.999997394009194,0.999997394009194,0.999997394009194,0.999997394009194,
0.999997394009194,0.999997394009194,0.999997394009194,0.999997394009194,
0.999997394009194,0.999997394009194,0.999997394009194,0.999997394009194,
0.999997394009194,0.999997394009194,0.999997394009194,0.999997394009194,
0.999997394009194,0.999997394009194,0.999997394009194,0.999997394009194,
0.999997394009194,0.999997394009194,0.999997394009194,0.999997394009194,
0.999997394009194,0.999997394009194,0.999997394009194,0.999997394009194,
0.999997394009194,0.999997394009194,0.999997394009194,0.999997394009194,
0.999997394009194,0.999997394009194,0.999997394009194,0.999997394009194,
0.999997394009194,0.999997394009194,0.999997394009194,0.999997394009194,
0.999997394009194,0.999997394009194,0.999997394009194,0.999997394009194,
0.999997394009194,0.999997394009194,0.999997394009194,0.999997394009194,
0.999997394009194,0.999997394009194,0.999997394009194,0.999997394009194,
0.999997394009194,0.999997394009194,0.999997394009194,0.999997394009194,
0.999997394009194,0.999997394009194,0.999997394009194,0.999997394009194,
0.999997394009194,0.999997394009194,0.999997394009194,0.999997394009194,
0.999997394009194,0.999997394009194,0.999997394009194,0.999997394009194,
0.999997394009194,0.999997394009194,0.999997394009194,0.999997394009194,
0.999997394009194,0.999997394009194,0.999997394009194,0.999997394009194,
0.999997394009194,0.999997394009194,0.999997394009194,0.999997394009194,
0.999997394009194,0.999997394009194,0.999997394009194,0.999997394009194,
0.999997394009194,0.999997394009194,0.999997394009194,0.999997394009194,
0.999997394009194,0.999997394009194,0.999997394009194,0.999997394009194,
0.999997394009194,0.999997394009194,0.999997394009194,0.999997394009194,
0.999997394009194,0.999997394009194,0.999997394009194,0.999997394009194,
0.999997394009194,0.999997394009194,0.999997394009194,0.999997394009194,
0.999997394009194,0.999997394009194,0.999997394009194,0.999997394009194,
0.999997394009194,0.999997394009194,0.999997394009194,0.999997394009194,
0.999997394009194,0.999997394009194,0.999997394009194,0.999997394009194,
0.999997394009194,0.999997394009194,0.999997394009194,0.999997394009194,
0.999997394009194,0.999997394009194,0.999997394009194,0.999997394009194,
0.999997394009194,0.999997394009194,0.999997394009194),(0.333333333333333,
0.333333333333333,0.333333333333333,0.333333333333333,0.333333333333333,
0.333333333333333,0.333333333333333,0.333333333333333,0.333333333333333,
0.333333333333333,0.333333333333333,0.333333333333333,0.333333333333333,
0.333333333333333,0.333333333333333,0.333333333333333,0.333333333333333,
0.333333333333333,0.333333333333333,0.333333333333333,0.333333333333333,
0.333333333333333,0.333333333333333,0.333333333333333,0.333333333333333,
0.333333333333333,0.333333333333333,0.333333333333333,0.333333333333333,
0.333333333333333,0.333333333333333,0.333333333333333,0.333333333333333,
0.333333333333333,0.333333333333333,0.333333333333333,0.333333333333333,
0.333333333333333,0.333333333333333,0.333333333333333,0.333333333333333,
0.333333333333333,0.333333333333333,0.333333333333333,0.333333333333333,
0.333333333333333,0.333333333333333,0.333333333333333,0.333333333333333,
0.333333333333333,0.333333333333333,0.333333333333333,0.333333333333333,
0.333333333333333,0.333333333333333,0.333333333333333,0.333333333333333,
0.333333333333333,0.333333333333333,0.333333333333333,0.333333333333333,
0.333333333333333,0.333333333333333,0.333333333333333,0.333333333333333,
0.333333333333333,0.333333333333333,0.333333333333333,0.333333333333333,
0.333333333333333,0.333333333333333,0.333333333333333,0.333333333333333,
0.333333333333333,0.333333333333333,0.333333333333333,0.333333333333333,
0.333333333333333,0.333333333333333,0.333333333333333,0.333333333333333,
0.333333333333333,0.333333333333333,0.333333333333333,0.333333333333333,
0.333333333333333,0.333333333333333,0.333333333333333,0.333333333333333,
0.333333333333333,0.333333333333333,0.333333333333333,0.333333333333333,
0.333333333333333,0.333333333333333,0.333333333333333,0.333333333333333,
0.333333333333333,0.333333333333333,0.333333333333333,0.333333333333333,
0.333333333333333,0.333333333333333,0.333333333333333,0.333333333333333,
0.333333333333333,0.333333333333333,0.333333333333333,0.333333333333333,
0.333333333333333,0.333333333333333,0.333333333333333,0.333333333333333,
0.333333333333333,0.333333333333333,0.333333333333333,0.333333333333333,
0.333333333333333,0.333333333333333,0.333333333333333,0.333333333333333,
0.333333333333333,0.333333333333333,0.333333333333333,0.333333333333333,
0.333333333333333,0.333333333333333,0.333333333333333,0.333333333333333,
0.333333333333333),(0.333333333333333,0.333333333333333,0.333333333333333,
0.333333333333333,0.333333333333333,0.333333333333333,0.333333333333333,
0.333333333333333,0.333333333333333,0.333333333333333,0.333333333333333,
0.333333333333333,0.333333333333333,0.333333333333333,0.333333333333333,
0.333333333333333,0.333333333333333,0.333333333333333,0.333333333333333,
0.333333333333333,0.333333333333333,0.333333333333333,0.333333333333333,
0.333333333333333,0.333333333333333,0.333333333333333,0.333333333333333,
0.333333333333333,0.333333333333333,0.333333333333333,0.333333333333333,
0.333333333333333,0.333333333333333,0.333333333333333,0.333333333333333,
0.333333333333333,0.333333333333333,0.333333333333333,0.333333333333333,
0.333333333333333,0.333333333333333,0.333333333333333,0.333333333333333,
0.333333333333333,0.333333333333333,0.333333333333333,0.333333333333333,
0.333333333333333,0.333333333333333,0.333333333333333,0.333333333333333,
0.333333333333333,0.333333333333333,0.333333333333333,0.333333333333333,
0.333333333333333,0.333333333333333,0.333333333333333,0.333333333333333,
0.333333333333333,0.333333333333333,0.333333333333333,0.333333333333333,
0.333333333333333,0.333333333333333,0.333333333333333,0.333333333333333,
0.333333333333333,0.333333333333333,0.333333333333333,0.333333333333333,
0.333333333333333,0.333333333333333,0.333333333333333,0.333333333333333,
0.333333333333333,0.333333333333333,0.333333333333333,0.333333333333333,
0.333333333333333,0.333333333333333,0.333333333333333,0.333333333333333,
0.333333333333333,0.333333333333333,0.333333333333333,0.333333333333333,
0.333333333333333,0.333333333333333,0.333333333333333,0.333333333333333,
0.333333333333333,0.333333333333333,0.333333333333333,0.333333333333333,
0.333333333333333,0.333333333333333,0.333333333333333,0.333333333333333,
0.333333333333333,0.333333333333333,0.333333333333333,0.333333333333333,
0.333333333333333,0.333333333333333,0.333333333333333,0.333333333333333,
0.333333333333333,0.333333333333333,0.333333333333333,0.333333333333333,
0.333333333333333,0.333333333333333,0.333333333333333,0.333333333333333,
0.333333333333333,0.333333333333333,0.333333333333333,0.333333333333333,
0.333333333333333,0.333333333333333,0.333333333333333,0.333333333333333,
0.333333333333333,0.333333333333333,0.333333333333333,0.333333333333333,
0.333333333333333,0.333333333333333,0.333333333333333),(1.,1.,1.,1.,1.,
1.,1.,1.,1.,1.,1.,1.,1.,1.,1.,1.,1.,1.,1.,1.,1.,1.,1.,1.,1.,1.,1.,1.,1.,
1.,1.,1.,1.,1.,1.,1.,1.,1.,1.,1.,1.,1.,1.,1.,1.,1.,1.,1.,1.,1.,1.,1.,1.,
1.,1.,1.,1.,1.,1.,1.,1.,1.,1.,1.,1.,1.,1.,1.,1.,1.,1.,1.,1.,1.,1.,1.,1.,
1.,1.,1.,1.,1.,1.,1.,1.,1.,1.,1.,1.,1.,1.,1.,1.,1.,1.,1.,1.,1.,1.,1.,1.,
1.,1.,1.,1.,1.,1.,1.,1.,1.,1.,1.,1.,1.,1.,1.,1.,1.,1.,1.,1.,1.,1.,1.,1.,
1.,1.,1.,1.,1.),(0.333334201998067,0.333334201998067,0.333334201998067,
0.333334201998067,0.333334201998067,0.333334201998067,0.333334201998067,
0.333334201998067,0.333334201998067,0.333334201998067,0.333334201998067,
0.333334201998067,0.333334201998067,0.333334201998067,0.333334201998067,
0.333334201998067,0.333334201998067,0.333334201998067,0.333334201998067,
0.333334201998067,0.333334201998067,0.333334201998067,0.333334201998067,
0.333334201998067,0.333334201998067,0.333334201998067,0.333334201998067,
0.333334201998067,0.333334201998067,0.333334201998067,0.333334201998067,
0.333334201998067,0.333334201998067,0.333334201998067,0.333334201998067,
0.333334201998067,0.333334201998067,0.333334201998067,0.333334201998067,
0.333334201998067,0.333334201998067,0.333334201998067,0.333334201998067,
0.333334201998067,0.333334201998067,0.333334201998067,0.333334201998067,
0.333334201998067,0.333334201998067,0.333334201998067,0.333334201998067,
0.333334201998067,0.333334201998067,0.333334201998067,0.333334201998067,
0.333334201998067,0.333334201998067,0.333334201998067,0.333334201998067,
0.333334201998067,0.333334201998067,0.333334201998067,0.333334201998067,
0.333334201998067,0.333334201998067,0.333334201998067,0.333334201998067,
0.333334201998067,0.333334201998067,0.333334201998067,0.333334201998067,
0.333334201998067,0.333334201998067,0.333334201998067,0.333334201998067,
0.333334201998067,0.333334201998067,0.333334201998067,0.333334201998067,
0.333334201998067,0.333334201998067,0.333334201998067,0.333334201998067,
0.333334201998067,0.333334201998067,0.333334201998067,0.333334201998067,
0.333334201998067,0.333334201998067,0.333334201998067,0.333334201998067,
0.333334201998067,0.333334201998067,0.333334201998067,0.333334201998067,
0.333334201998067,0.333334201998067,0.333334201998067,0.333334201998067,
0.333334201998067,0.333334201998067,0.333334201998067,0.333334201998067,
0.333334201998067,0.333334201998067,0.333334201998067,0.333334201998067,
0.333334201998067,0.333334201998067,0.333334201998067,0.333334201998067,
0.333334201998067,0.333334201998067,0.333334201998067,0.333334201998067,
0.333334201998067,0.333334201998067,0.333334201998067,0.333334201998067,
0.333334201998067,0.333334201998067,0.333334201998067,0.333334201998067,
0.333334201998067,0.333334201998067,0.333334201998067,0.333334201998067,
0.333334201998067,0.333334201998067,0.333334201998067),(0.333333333334465,
0.333333333334465,0.333333333334465,0.333333333334465,0.333333333334465,
0.333333333334465,0.333333333334465,0.333333333334465,0.333333333334465,
0.333333333334465,0.333333333334465,0.333333333334465,0.333333333334465,
0.333333333334465,0.333333333334465,0.333333333334465,0.333333333334465,
0.333333333334465,0.333333333334465,0.333333333334465,0.333333333334465,
0.333333333334465,0.333333333334465,0.333333333334465,0.333333333334465,
0.333333333334465,0.333333333334465,0.333333333334465,0.333333333334465,
0.333333333334465,0.333333333334465,0.333333333334465,0.333333333334465,
0.333333333334465,0.333333333334465,0.333333333334465,0.333333333334465,
0.333333333334465,0.333333333334465,0.333333333334465,0.333333333334465,
0.333333333334465,0.333333333334465,0.333333333334465,0.333333333334465,
0.333333333334465,0.333333333334465,0.333333333334465,0.333333333334465,
0.333333333334465,0.333333333334465,0.333333333334465,0.333333333334465,
0.333333333334465,0.333333333334465,0.333333333334465,0.333333333334465,
0.333333333334465,0.333333333334465,0.333333333334465,0.333333333334465,
0.333333333334465,0.333333333334465,0.333333333334465,0.333333333334465,
0.333333333334465,0.333333333334465,0.333333333334465,0.333333333334465,
0.333333333334465,0.333333333334465,0.333333333334465,0.333333333334465,
0.333333333334465,0.333333333334465,0.333333333334465,0.333333333334465,
0.333333333334465,0.333333333334465,0.333333333334465,0.333333333334465,
0.333333333334465,0.333333333334465,0.333333333334465,0.333333333334465,
0.333333333334465,0.333333333334465,0.333333333334465,0.333333333334465,
0.333333333334465,0.333333333334465,0.333333333334465,0.333333333334465,
0.333333333334465,0.333333333334465,0.333333333334465,0.333333333334465,
0.333333333334465,0.333333333334465,0.333333333334465,0.333333333334465,
0.333333333334465,0.333333333334465,0.333333333334465,0.333333333334465,
0.333333333334465,0.333333333334465,0.333333333334465,0.333333333334465,
0.333333333334465,0.333333333334465,0.333333333334465,0.333333333334465,
0.333333333334465,0.333333333334465,0.333333333334465,0.333333333334465,
0.333333333334465,0.333333333334465,0.333333333334465,0.333333333334465,
0.333333333334465,0.333333333334465,0.333333333334465,0.333333333334465,
0.333333333334465,0.333333333334465,0.333333333334465,0.333333333334465,
0.333333333334465),(0.999997394009194,0.999997394009194,0.999997394009194,
0.999997394009194,0.999997394009194,0.999997394009194,0.999997394009194,
0.999997394009194,0.999997394009194,0.999997394009194,0.999997394009194,
0.999997394009194,0.999997394009194,0.999997394009194,0.999997394009194,
0.999997394009194,0.999997394009194,0.999997394009194,0.999997394009194,
0.999997394009194,0.999997394009194,0.999997394009194,0.999997394009194,
0.999997394009194,0.999997394009194,0.999997394009194,0.999997394009194,
0.999997394009194,0.999997394009194,0.999997394009194,0.999997394009194,
0.999997394009194,0.999997394009194,0.999997394009194,0.999997394009194,
0.999997394009194,0.999997394009194,0.999997394009194,0.999997394009194,
0.999997394009194,0.999997394009194,0.999997394009194,0.999997394009194,
0.999997394009194,0.999997394009194,0.999997394009194,0.999997394009194,
0.999997394009194,0.999997394009194,0.999997394009194,0.999997394009194,
0.999997394009194,0.999997394009194,0.999997394009194,0.999997394009194,
0.999997394009194,0.999997394009194,0.999997394009194,0.999997394009194,
0.999997394009194,0.999997394009194,0.999997394009194,0.999997394009194,
0.999997394009194,0.999997394009194,0.999997394009194,0.999997394009194,
0.999997394009194,0.999997394009194,0.999997394009194,0.999997394009194,
0.999997394009194,0.999997394009194,0.999997394009194,0.999997394009194,
0.999997394009194,0.999997394009194,0.999997394009194,0.999997394009194,
0.999997394009194,0.999997394009194,0.999997394009194,0.999997394009194,
0.999997394009194,0.999997394009194,0.999997394009194,0.999997394009194,
0.999997394009194,0.999997394009194,0.999997394009194,0.999997394009194,
0.999997394009194,0.999997394009194,0.999997394009194,0.999997394009194,
0.999997394009194,0.999997394009194,0.999997394009194,0.999997394009194,
0.999997394009194,0.999997394009194,0.999997394009194,0.999997394009194,
0.999997394009194,0.999997394009194,0.999997394009194,0.999997394009194,
0.999997394009194,0.999997394009194,0.999997394009194,0.999997394009194,
0.999997394009194,0.999997394009194,0.999997394009194,0.999997394009194,
0.999997394009194,0.999997394009194,0.999997394009194,0.999997394009194,
0.999997394009194,0.999997394009194,0.999997394009194,0.999997394009194,
0.999997394009194,0.999997394009194,0.999997394009194,0.999997394009194,
0.999997394009194,0.999997394009194,0.999997394009194)))
REPRESENTATION_ITEM('')
SURFACE()
);
#61=(
BOUNDED_SURFACE()
B_SPLINE_SURFACE(3,3,((#3765,#3766,#3767,#3768,#3769,#3770,#3771,#3772,
#3773,#3774,#3775,#3776,#3777,#3778,#3779,#3780,#3781,#3782,#3783,#3784,
#3785,#3786,#3787,#3788,#3789,#3790,#3791,#3792,#3793,#3794,#3795,#3796,
#3797,#3798,#3799,#3800,#3801,#3802,#3803,#3804,#3805,#3806,#3807,#3808,
#3809,#3810,#3811,#3812,#3813,#3814,#3815,#3816,#3817,#3818,#3819,#3820,
#3821,#3822,#3823,#3824,#3825,#3826,#3827,#3828,#3829,#3830,#3831,#3832,
#3833,#3834,#3835,#3836,#3837,#3838,#3839,#3840,#3841,#3842,#3843,#3844,
#3845,#3846,#3847,#3848,#3849,#3850,#3851,#3852,#3853,#3854,#3855,#3856,
#3857,#3858,#3859,#3860,#3861,#3862,#3863,#3864,#3865,#3866,#3867,#3868,
#3869,#3870,#3871,#3872,#3873,#3874,#3875,#3876,#3877,#3878,#3879,#3880,
#3881,#3882,#3883,#3884,#3885,#3886,#3887,#3888,#3889,#3890,#3891,#3892,
#3893,#3894),(#3895,#3896,#3897,#3898,#3899,#3900,#3901,#3902,#3903,#3904,
#3905,#3906,#3907,#3908,#3909,#3910,#3911,#3912,#3913,#3914,#3915,#3916,
#3917,#3918,#3919,#3920,#3921,#3922,#3923,#3924,#3925,#3926,#3927,#3928,
#3929,#3930,#3931,#3932,#3933,#3934,#3935,#3936,#3937,#3938,#3939,#3940,
#3941,#3942,#3943,#3944,#3945,#3946,#3947,#3948,#3949,#3950,#3951,#3952,
#3953,#3954,#3955,#3956,#3957,#3958,#3959,#3960,#3961,#3962,#3963,#3964,
#3965,#3966,#3967,#3968,#3969,#3970,#3971,#3972,#3973,#3974,#3975,#3976,
#3977,#3978,#3979,#3980,#3981,#3982,#3983,#3984,#3985,#3986,#3987,#3988,
#3989,#3990,#3991,#3992,#3993,#3994,#3995,#3996,#3997,#3998,#3999,#4000,
#4001,#4002,#4003,#4004,#4005,#4006,#4007,#4008,#4009,#4010,#4011,#4012,
#4013,#4014,#4015,#4016,#4017,#4018,#4019,#4020,#4021,#4022,#4023,#4024),
(#4025,#4026,#4027,#4028,#4029,#4030,#4031,#4032,#4033,#4034,#4035,#4036,
#4037,#4038,#4039,#4040,#4041,#4042,#4043,#4044,#4045,#4046,#4047,#4048,
#4049,#4050,#4051,#4052,#4053,#4054,#4055,#4056,#4057,#4058,#4059,#4060,
#4061,#4062,#4063,#4064,#4065,#4066,#4067,#4068,#4069,#4070,#4071,#4072,
#4073,#4074,#4075,#4076,#4077,#4078,#4079,#4080,#4081,#4082,#4083,#4084,
#4085,#4086,#4087,#4088,#4089,#4090,#4091,#4092,#4093,#4094,#4095,#4096,
#4097,#4098,#4099,#4100,#4101,#4102,#4103,#4104,#4105,#4106,#4107,#4108,
#4109,#4110,#4111,#4112,#4113,#4114,#4115,#4116,#4117,#4118,#4119,#4120,
#4121,#4122,#4123,#4124,#4125,#4126,#4127,#4128,#4129,#4130,#4131,#4132,
#4133,#4134,#4135,#4136,#4137,#4138,#4139,#4140,#4141,#4142,#4143,#4144,
#4145,#4146,#4147,#4148,#4149,#4150,#4151,#4152,#4153,#4154),(#4155,#4156,
#4157,#4158,#4159,#4160,#4161,#4162,#4163,#4164,#4165,#4166,#4167,#4168,
#4169,#4170,#4171,#4172,#4173,#4174,#4175,#4176,#4177,#4178,#4179,#4180,
#4181,#4182,#4183,#4184,#4185,#4186,#4187,#4188,#4189,#4190,#4191,#4192,
#4193,#4194,#4195,#4196,#4197,#4198,#4199,#4200,#4201,#4202,#4203,#4204,
#4205,#4206,#4207,#4208,#4209,#4210,#4211,#4212,#4213,#4214,#4215,#4216,
#4217,#4218,#4219,#4220,#4221,#4222,#4223,#4224,#4225,#4226,#4227,#4228,
#4229,#4230,#4231,#4232,#4233,#4234,#4235,#4236,#4237,#4238,#4239,#4240,
#4241,#4242,#4243,#4244,#4245,#4246,#4247,#4248,#4249,#4250,#4251,#4252,
#4253,#4254,#4255,#4256,#4257,#4258,#4259,#4260,#4261,#4262,#4263,#4264,
#4265,#4266,#4267,#4268,#4269,#4270,#4271,#4272,#4273,#4274,#4275,#4276,
#4277,#4278,#4279,#4280,#4281,#4282,#4283,#4284),(#4285,#4286,#4287,#4288,
#4289,#4290,#4291,#4292,#4293,#4294,#4295,#4296,#4297,#4298,#4299,#4300,
#4301,#4302,#4303,#4304,#4305,#4306,#4307,#4308,#4309,#4310,#4311,#4312,
#4313,#4314,#4315,#4316,#4317,#4318,#4319,#4320,#4321,#4322,#4323,#4324,
#4325,#4326,#4327,#4328,#4329,#4330,#4331,#4332,#4333,#4334,#4335,#4336,
#4337,#4338,#4339,#4340,#4341,#4342,#4343,#4344,#4345,#4346,#4347,#4348,
#4349,#4350,#4351,#4352,#4353,#4354,#4355,#4356,#4357,#4358,#4359,#4360,
#4361,#4362,#4363,#4364,#4365,#4366,#4367,#4368,#4369,#4370,#4371,#4372,
#4373,#4374,#4375,#4376,#4377,#4378,#4379,#4380,#4381,#4382,#4383,#4384,
#4385,#4386,#4387,#4388,#4389,#4390,#4391,#4392,#4393,#4394,#4395,#4396,
#4397,#4398,#4399,#4400,#4401,#4402,#4403,#4404,#4405,#4406,#4407,#4408,
#4409,#4410,#4411,#4412,#4413,#4414),(#4415,#4416,#4417,#4418,#4419,#4420,
#4421,#4422,#4423,#4424,#4425,#4426,#4427,#4428,#4429,#4430,#4431,#4432,
#4433,#4434,#4435,#4436,#4437,#4438,#4439,#4440,#4441,#4442,#4443,#4444,
#4445,#4446,#4447,#4448,#4449,#4450,#4451,#4452,#4453,#4454,#4455,#4456,
#4457,#4458,#4459,#4460,#4461,#4462,#4463,#4464,#4465,#4466,#4467,#4468,
#4469,#4470,#4471,#4472,#4473,#4474,#4475,#4476,#4477,#4478,#4479,#4480,
#4481,#4482,#4483,#4484,#4485,#4486,#4487,#4488,#4489,#4490,#4491,#4492,
#4493,#4494,#4495,#4496,#4497,#4498,#4499,#4500,#4501,#4502,#4503,#4504,
#4505,#4506,#4507,#4508,#4509,#4510,#4511,#4512,#4513,#4514,#4515,#4516,
#4517,#4518,#4519,#4520,#4521,#4522,#4523,#4524,#4525,#4526,#4527,#4528,
#4529,#4530,#4531,#4532,#4533,#4534,#4535,#4536,#4537,#4538,#4539,#4540,
#4541,#4542,#4543,#4544),(#4545,#4546,#4547,#4548,#4549,#4550,#4551,#4552,
#4553,#4554,#4555,#4556,#4557,#4558,#4559,#4560,#4561,#4562,#4563,#4564,
#4565,#4566,#4567,#4568,#4569,#4570,#4571,#4572,#4573,#4574,#4575,#4576,
#4577,#4578,#4579,#4580,#4581,#4582,#4583,#4584,#4585,#4586,#4587,#4588,
#4589,#4590,#4591,#4592,#4593,#4594,#4595,#4596,#4597,#4598,#4599,#4600,
#4601,#4602,#4603,#4604,#4605,#4606,#4607,#4608,#4609,#4610,#4611,#4612,
#4613,#4614,#4615,#4616,#4617,#4618,#4619,#4620,#4621,#4622,#4623,#4624,
#4625,#4626,#4627,#4628,#4629,#4630,#4631,#4632,#4633,#4634,#4635,#4636,
#4637,#4638,#4639,#4640,#4641,#4642,#4643,#4644,#4645,#4646,#4647,#4648,
#4649,#4650,#4651,#4652,#4653,#4654,#4655,#4656,#4657,#4658,#4659,#4660,
#4661,#4662,#4663,#4664,#4665,#4666,#4667,#4668,#4669,#4670,#4671,#4672,
#4673,#4674)),.UNSPECIFIED.,.T.,.F.,.F.)
B_SPLINE_SURFACE_WITH_KNOTS((4,3,4),(4,2,2,2,2,2,2,2,2,2,2,2,2,2,2,2,2,
2,2,2,2,2,2,2,2,2,2,2,2,2,2,2,2,2,2,2,2,2,2,2,2,2,2,2,2,2,2,2,2,2,2,2,2,
2,2,2,2,2,2,2,2,2,2,2,4),(0.499999335657285,1.,1.49999933565728),(0.,0.015625,
0.03125,0.046875,0.0625,0.078125,0.09375,0.109375,0.125,0.140625,0.15625,
0.171875,0.1875,0.203125,0.21875,0.234375,0.25,0.265625,0.28125,0.296875,
0.3125,0.328125,0.34375,0.359375,0.375,0.390625,0.40625,0.421875,0.4375,
0.453125,0.46875,0.484375,0.5,0.515625,0.53125,0.546875,0.5625,0.578125,
0.59375,0.609375,0.625,0.640625,0.65625,0.671875,0.6875,0.703125,0.71875,
0.734375,0.75,0.765625,0.78125,0.796875,0.8125,0.828125,0.84375,0.859375,
0.875,0.890625,0.90625,0.921875,0.9375,0.953125,0.96875,0.984375,1.),
 .UNSPECIFIED.)
GEOMETRIC_REPRESENTATION_ITEM()
RATIONAL_B_SPLINE_SURFACE(((0.999997342632669,0.999997342632669,0.999997342632669,
0.999997342632669,0.999997342632669,0.999997342632669,0.999997342632669,
0.999997342632669,0.999997342632669,0.999997342632669,0.999997342632669,
0.999997342632669,0.999997342632669,0.999997342632669,0.999997342632669,
0.999997342632669,0.999997342632669,0.999997342632669,0.999997342632669,
0.999997342632669,0.999997342632669,0.999997342632669,0.999997342632669,
0.999997342632669,0.999997342632669,0.999997342632669,0.999997342632669,
0.999997342632669,0.999997342632669,0.999997342632669,0.999997342632669,
0.999997342632669,0.999997342632669,0.999997342632669,0.999997342632669,
0.999997342632669,0.999997342632669,0.999997342632669,0.999997342632669,
0.999997342632669,0.999997342632669,0.999997342632669,0.999997342632669,
0.999997342632669,0.999997342632669,0.999997342632669,0.999997342632669,
0.999997342632669,0.999997342632669,0.999997342632669,0.999997342632669,
0.999997342632669,0.999997342632669,0.999997342632669,0.999997342632669,
0.999997342632669,0.999997342632669,0.999997342632669,0.999997342632669,
0.999997342632669,0.999997342632669,0.999997342632669,0.999997342632669,
0.999997342632669,0.999997342632669,0.999997342632669,0.999997342632669,
0.999997342632669,0.999997342632669,0.999997342632669,0.999997342632669,
0.999997342632669,0.999997342632669,0.999997342632669,0.999997342632669,
0.999997342632669,0.999997342632669,0.999997342632669,0.999997342632669,
0.999997342632669,0.999997342632669,0.999997342632669,0.999997342632669,
0.999997342632669,0.999997342632669,0.999997342632669,0.999997342632669,
0.999997342632669,0.999997342632669,0.999997342632669,0.999997342632669,
0.999997342632669,0.999997342632669,0.999997342632669,0.999997342632669,
0.999997342632669,0.999997342632669,0.999997342632669,0.999997342632669,
0.999997342632669,0.999997342632669,0.999997342632669,0.999997342632669,
0.999997342632669,0.999997342632669,0.999997342632669,0.999997342632669,
0.999997342632669,0.999997342632669,0.999997342632669,0.999997342632669,
0.999997342632669,0.999997342632669,0.999997342632669,0.999997342632669,
0.999997342632669,0.999997342632669,0.999997342632669,0.999997342632669,
0.999997342632669,0.999997342632669,0.999997342632669,0.999997342632669,
0.999997342632669,0.999997342632669,0.999997342632669,0.999997342632669,
0.999997342632669,0.999997342632669,0.999997342632669),(0.333333333333333,
0.333333333333333,0.333333333333333,0.333333333333333,0.333333333333333,
0.333333333333333,0.333333333333333,0.333333333333333,0.333333333333333,
0.333333333333333,0.333333333333333,0.333333333333333,0.333333333333333,
0.333333333333333,0.333333333333333,0.333333333333333,0.333333333333333,
0.333333333333333,0.333333333333333,0.333333333333333,0.333333333333333,
0.333333333333333,0.333333333333333,0.333333333333333,0.333333333333333,
0.333333333333333,0.333333333333333,0.333333333333333,0.333333333333333,
0.333333333333333,0.333333333333333,0.333333333333333,0.333333333333333,
0.333333333333333,0.333333333333333,0.333333333333333,0.333333333333333,
0.333333333333333,0.333333333333333,0.333333333333333,0.333333333333333,
0.333333333333333,0.333333333333333,0.333333333333333,0.333333333333333,
0.333333333333333,0.333333333333333,0.333333333333333,0.333333333333333,
0.333333333333333,0.333333333333333,0.333333333333333,0.333333333333333,
0.333333333333333,0.333333333333333,0.333333333333333,0.333333333333333,
0.333333333333333,0.333333333333333,0.333333333333333,0.333333333333333,
0.333333333333333,0.333333333333333,0.333333333333333,0.333333333333333,
0.333333333333333,0.333333333333333,0.333333333333333,0.333333333333333,
0.333333333333333,0.333333333333333,0.333333333333333,0.333333333333333,
0.333333333333333,0.333333333333333,0.333333333333333,0.333333333333333,
0.333333333333333,0.333333333333333,0.333333333333333,0.333333333333333,
0.333333333333333,0.333333333333333,0.333333333333333,0.333333333333333,
0.333333333333333,0.333333333333333,0.333333333333333,0.333333333333333,
0.333333333333333,0.333333333333333,0.333333333333333,0.333333333333333,
0.333333333333333,0.333333333333333,0.333333333333333,0.333333333333333,
0.333333333333333,0.333333333333333,0.333333333333333,0.333333333333333,
0.333333333333333,0.333333333333333,0.333333333333333,0.333333333333333,
0.333333333333333,0.333333333333333,0.333333333333333,0.333333333333333,
0.333333333333333,0.333333333333333,0.333333333333333,0.333333333333333,
0.333333333333333,0.333333333333333,0.333333333333333,0.333333333333333,
0.333333333333333,0.333333333333333,0.333333333333333,0.333333333333333,
0.333333333333333,0.333333333333333,0.333333333333333,0.333333333333333,
0.333333333333333,0.333333333333333,0.333333333333333,0.333333333333333,
0.333333333333333),(0.333333333333333,0.333333333333333,0.333333333333333,
0.333333333333333,0.333333333333333,0.333333333333333,0.333333333333333,
0.333333333333333,0.333333333333333,0.333333333333333,0.333333333333333,
0.333333333333333,0.333333333333333,0.333333333333333,0.333333333333333,
0.333333333333333,0.333333333333333,0.333333333333333,0.333333333333333,
0.333333333333333,0.333333333333333,0.333333333333333,0.333333333333333,
0.333333333333333,0.333333333333333,0.333333333333333,0.333333333333333,
0.333333333333333,0.333333333333333,0.333333333333333,0.333333333333333,
0.333333333333333,0.333333333333333,0.333333333333333,0.333333333333333,
0.333333333333333,0.333333333333333,0.333333333333333,0.333333333333333,
0.333333333333333,0.333333333333333,0.333333333333333,0.333333333333333,
0.333333333333333,0.333333333333333,0.333333333333333,0.333333333333333,
0.333333333333333,0.333333333333333,0.333333333333333,0.333333333333333,
0.333333333333333,0.333333333333333,0.333333333333333,0.333333333333333,
0.333333333333333,0.333333333333333,0.333333333333333,0.333333333333333,
0.333333333333333,0.333333333333333,0.333333333333333,0.333333333333333,
0.333333333333333,0.333333333333333,0.333333333333333,0.333333333333333,
0.333333333333333,0.333333333333333,0.333333333333333,0.333333333333333,
0.333333333333333,0.333333333333333,0.333333333333333,0.333333333333333,
0.333333333333333,0.333333333333333,0.333333333333333,0.333333333333333,
0.333333333333333,0.333333333333333,0.333333333333333,0.333333333333333,
0.333333333333333,0.333333333333333,0.333333333333333,0.333333333333333,
0.333333333333333,0.333333333333333,0.333333333333333,0.333333333333333,
0.333333333333333,0.333333333333333,0.333333333333333,0.333333333333333,
0.333333333333333,0.333333333333333,0.333333333333333,0.333333333333333,
0.333333333333333,0.333333333333333,0.333333333333333,0.333333333333333,
0.333333333333333,0.333333333333333,0.333333333333333,0.333333333333333,
0.333333333333333,0.333333333333333,0.333333333333333,0.333333333333333,
0.333333333333333,0.333333333333333,0.333333333333333,0.333333333333333,
0.333333333333333,0.333333333333333,0.333333333333333,0.333333333333333,
0.333333333333333,0.333333333333333,0.333333333333333,0.333333333333333,
0.333333333333333,0.333333333333333,0.333333333333333,0.333333333333333,
0.333333333333333,0.333333333333333,0.333333333333333),(1.,1.,1.,1.,1.,
1.,1.,1.,1.,1.,1.,1.,1.,1.,1.,1.,1.,1.,1.,1.,1.,1.,1.,1.,1.,1.,1.,1.,1.,
1.,1.,1.,1.,1.,1.,1.,1.,1.,1.,1.,1.,1.,1.,1.,1.,1.,1.,1.,1.,1.,1.,1.,1.,
1.,1.,1.,1.,1.,1.,1.,1.,1.,1.,1.,1.,1.,1.,1.,1.,1.,1.,1.,1.,1.,1.,1.,1.,
1.,1.,1.,1.,1.,1.,1.,1.,1.,1.,1.,1.,1.,1.,1.,1.,1.,1.,1.,1.,1.,1.,1.,1.,
1.,1.,1.,1.,1.,1.,1.,1.,1.,1.,1.,1.,1.,1.,1.,1.,1.,1.,1.,1.,1.,1.,1.,1.,
1.,1.,1.,1.,1.),(0.333334219123621,0.333334219123621,0.333334219123621,
0.333334219123621,0.333334219123621,0.333334219123621,0.333334219123621,
0.333334219123621,0.333334219123621,0.333334219123621,0.333334219123621,
0.333334219123621,0.333334219123621,0.333334219123621,0.333334219123621,
0.333334219123621,0.333334219123621,0.333334219123621,0.333334219123621,
0.333334219123621,0.333334219123621,0.333334219123621,0.333334219123621,
0.333334219123621,0.333334219123621,0.333334219123621,0.333334219123621,
0.333334219123621,0.333334219123621,0.333334219123621,0.333334219123621,
0.333334219123621,0.333334219123621,0.333334219123621,0.333334219123621,
0.333334219123621,0.333334219123621,0.333334219123621,0.333334219123621,
0.333334219123621,0.333334219123621,0.333334219123621,0.333334219123621,
0.333334219123621,0.333334219123621,0.333334219123621,0.333334219123621,
0.333334219123621,0.333334219123621,0.333334219123621,0.333334219123621,
0.333334219123621,0.333334219123621,0.333334219123621,0.333334219123621,
0.333334219123621,0.333334219123621,0.333334219123621,0.333334219123621,
0.333334219123621,0.333334219123621,0.333334219123621,0.333334219123621,
0.333334219123621,0.333334219123621,0.333334219123621,0.333334219123621,
0.333334219123621,0.333334219123621,0.333334219123621,0.333334219123621,
0.333334219123621,0.333334219123621,0.333334219123621,0.333334219123621,
0.333334219123621,0.333334219123621,0.333334219123621,0.333334219123621,
0.333334219123621,0.333334219123621,0.333334219123621,0.333334219123621,
0.333334219123621,0.333334219123621,0.333334219123621,0.333334219123621,
0.333334219123621,0.333334219123621,0.333334219123621,0.333334219123621,
0.333334219123621,0.333334219123621,0.333334219123621,0.333334219123621,
0.333334219123621,0.333334219123621,0.333334219123621,0.333334219123621,
0.333334219123621,0.333334219123621,0.333334219123621,0.333334219123621,
0.333334219123621,0.333334219123621,0.333334219123621,0.333334219123621,
0.333334219123621,0.333334219123621,0.333334219123621,0.333334219123621,
0.333334219123621,0.333334219123621,0.333334219123621,0.333334219123621,
0.333334219123621,0.333334219123621,0.333334219123621,0.333334219123621,
0.333334219123621,0.333334219123621,0.333334219123621,0.333334219123621,
0.333334219123621,0.333334219123621,0.333334219123621,0.333334219123621,
0.333334219123621,0.333334219123621,0.333334219123621),(0.33333333333451,
0.33333333333451,0.33333333333451,0.33333333333451,0.33333333333451,0.33333333333451,
0.33333333333451,0.33333333333451,0.33333333333451,0.33333333333451,0.33333333333451,
0.33333333333451,0.33333333333451,0.33333333333451,0.33333333333451,0.33333333333451,
0.33333333333451,0.33333333333451,0.33333333333451,0.33333333333451,0.33333333333451,
0.33333333333451,0.33333333333451,0.33333333333451,0.33333333333451,0.33333333333451,
0.33333333333451,0.33333333333451,0.33333333333451,0.33333333333451,0.33333333333451,
0.33333333333451,0.33333333333451,0.33333333333451,0.33333333333451,0.33333333333451,
0.33333333333451,0.33333333333451,0.33333333333451,0.33333333333451,0.33333333333451,
0.33333333333451,0.33333333333451,0.33333333333451,0.33333333333451,0.33333333333451,
0.33333333333451,0.33333333333451,0.33333333333451,0.33333333333451,0.33333333333451,
0.33333333333451,0.33333333333451,0.33333333333451,0.33333333333451,0.33333333333451,
0.33333333333451,0.33333333333451,0.33333333333451,0.33333333333451,0.33333333333451,
0.33333333333451,0.33333333333451,0.33333333333451,0.33333333333451,0.33333333333451,
0.33333333333451,0.33333333333451,0.33333333333451,0.33333333333451,0.33333333333451,
0.33333333333451,0.33333333333451,0.33333333333451,0.33333333333451,0.33333333333451,
0.33333333333451,0.33333333333451,0.33333333333451,0.33333333333451,0.33333333333451,
0.33333333333451,0.33333333333451,0.33333333333451,0.33333333333451,0.33333333333451,
0.33333333333451,0.33333333333451,0.33333333333451,0.33333333333451,0.33333333333451,
0.33333333333451,0.33333333333451,0.33333333333451,0.33333333333451,0.33333333333451,
0.33333333333451,0.33333333333451,0.33333333333451,0.33333333333451,0.33333333333451,
0.33333333333451,0.33333333333451,0.33333333333451,0.33333333333451,0.33333333333451,
0.33333333333451,0.33333333333451,0.33333333333451,0.33333333333451,0.33333333333451,
0.33333333333451,0.33333333333451,0.33333333333451,0.33333333333451,0.33333333333451,
0.33333333333451,0.33333333333451,0.33333333333451,0.33333333333451,0.33333333333451,
0.33333333333451,0.33333333333451,0.33333333333451,0.33333333333451,0.33333333333451,
0.33333333333451,0.33333333333451,0.33333333333451,0.33333333333451),(0.999997342632669,
0.999997342632669,0.999997342632669,0.999997342632669,0.999997342632669,
0.999997342632669,0.999997342632669,0.999997342632669,0.999997342632669,
0.999997342632669,0.999997342632669,0.999997342632669,0.999997342632669,
0.999997342632669,0.999997342632669,0.999997342632669,0.999997342632669,
0.999997342632669,0.999997342632669,0.999997342632669,0.999997342632669,
0.999997342632669,0.999997342632669,0.999997342632669,0.999997342632669,
0.999997342632669,0.999997342632669,0.999997342632669,0.999997342632669,
0.999997342632669,0.999997342632669,0.999997342632669,0.999997342632669,
0.999997342632669,0.999997342632669,0.999997342632669,0.999997342632669,
0.999997342632669,0.999997342632669,0.999997342632669,0.999997342632669,
0.999997342632669,0.999997342632669,0.999997342632669,0.999997342632669,
0.999997342632669,0.999997342632669,0.999997342632669,0.999997342632669,
0.999997342632669,0.999997342632669,0.999997342632669,0.999997342632669,
0.999997342632669,0.999997342632669,0.999997342632669,0.999997342632669,
0.999997342632669,0.999997342632669,0.999997342632669,0.999997342632669,
0.999997342632669,0.999997342632669,0.999997342632669,0.999997342632669,
0.999997342632669,0.999997342632669,0.999997342632669,0.999997342632669,
0.999997342632669,0.999997342632669,0.999997342632669,0.999997342632669,
0.999997342632669,0.999997342632669,0.999997342632669,0.999997342632669,
0.999997342632669,0.999997342632669,0.999997342632669,0.999997342632669,
0.999997342632669,0.999997342632669,0.999997342632669,0.999997342632669,
0.999997342632669,0.999997342632669,0.999997342632669,0.999997342632669,
0.999997342632669,0.999997342632669,0.999997342632669,0.999997342632669,
0.999997342632669,0.999997342632669,0.999997342632669,0.999997342632669,
0.999997342632669,0.999997342632669,0.999997342632669,0.999997342632669,
0.999997342632669,0.999997342632669,0.999997342632669,0.999997342632669,
0.999997342632669,0.999997342632669,0.999997342632669,0.999997342632669,
0.999997342632669,0.999997342632669,0.999997342632669,0.999997342632669,
0.999997342632669,0.999997342632669,0.999997342632669,0.999997342632669,
0.999997342632669,0.999997342632669,0.999997342632669,0.999997342632669,
0.999997342632669,0.999997342632669,0.999997342632669,0.999997342632669,
0.999997342632669,0.999997342632669,0.999997342632669,0.999997342632669,
0.999997342632669)))
REPRESENTATION_ITEM('')
SURFACE()
);
#62=(
BOUNDED_SURFACE()
B_SPLINE_SURFACE(3,3,((#4678,#4679,#4680,#4681,#4682,#4683,#4684,#4685,
#4686,#4687,#4688,#4689,#4690,#4691,#4692,#4693,#4694,#4695,#4696,#4697,
#4698,#4699,#4700,#4701,#4702,#4703,#4704,#4705,#4706,#4707,#4708,#4709,
#4710,#4711,#4712,#4713,#4714,#4715,#4716,#4717,#4718,#4719,#4720,#4721,
#4722,#4723,#4724,#4725,#4726,#4727,#4728,#4729,#4730,#4731,#4732,#4733,
#4734,#4735,#4736,#4737,#4738,#4739,#4740,#4741,#4742,#4743,#4744,#4745,
#4746,#4747,#4748,#4749,#4750,#4751,#4752,#4753,#4754,#4755,#4756,#4757,
#4758,#4759,#4760,#4761,#4762,#4763,#4764,#4765,#4766,#4767,#4768,#4769,
#4770,#4771,#4772,#4773,#4774,#4775,#4776,#4777,#4778,#4779,#4780,#4781),
(#4782,#4783,#4784,#4785,#4786,#4787,#4788,#4789,#4790,#4791,#4792,#4793,
#4794,#4795,#4796,#4797,#4798,#4799,#4800,#4801,#4802,#4803,#4804,#4805,
#4806,#4807,#4808,#4809,#4810,#4811,#4812,#4813,#4814,#4815,#4816,#4817,
#4818,#4819,#4820,#4821,#4822,#4823,#4824,#4825,#4826,#4827,#4828,#4829,
#4830,#4831,#4832,#4833,#4834,#4835,#4836,#4837,#4838,#4839,#4840,#4841,
#4842,#4843,#4844,#4845,#4846,#4847,#4848,#4849,#4850,#4851,#4852,#4853,
#4854,#4855,#4856,#4857,#4858,#4859,#4860,#4861,#4862,#4863,#4864,#4865,
#4866,#4867,#4868,#4869,#4870,#4871,#4872,#4873,#4874,#4875,#4876,#4877,
#4878,#4879,#4880,#4881,#4882,#4883,#4884,#4885),(#4886,#4887,#4888,#4889,
#4890,#4891,#4892,#4893,#4894,#4895,#4896,#4897,#4898,#4899,#4900,#4901,
#4902,#4903,#4904,#4905,#4906,#4907,#4908,#4909,#4910,#4911,#4912,#4913,
#4914,#4915,#4916,#4917,#4918,#4919,#4920,#4921,#4922,#4923,#4924,#4925,
#4926,#4927,#4928,#4929,#4930,#4931,#4932,#4933,#4934,#4935,#4936,#4937,
#4938,#4939,#4940,#4941,#4942,#4943,#4944,#4945,#4946,#4947,#4948,#4949,
#4950,#4951,#4952,#4953,#4954,#4955,#4956,#4957,#4958,#4959,#4960,#4961,
#4962,#4963,#4964,#4965,#4966,#4967,#4968,#4969,#4970,#4971,#4972,#4973,
#4974,#4975,#4976,#4977,#4978,#4979,#4980,#4981,#4982,#4983,#4984,#4985,
#4986,#4987,#4988,#4989),(#4990,#4991,#4992,#4993,#4994,#4995,#4996,#4997,
#4998,#4999,#5000,#5001,#5002,#5003,#5004,#5005,#5006,#5007,#5008,#5009,
#5010,#5011,#5012,#5013,#5014,#5015,#5016,#5017,#5018,#5019,#5020,#5021,
#5022,#5023,#5024,#5025,#5026,#5027,#5028,#5029,#5030,#5031,#5032,#5033,
#5034,#5035,#5036,#5037,#5038,#5039,#5040,#5041,#5042,#5043,#5044,#5045,
#5046,#5047,#5048,#5049,#5050,#5051,#5052,#5053,#5054,#5055,#5056,#5057,
#5058,#5059,#5060,#5061,#5062,#5063,#5064,#5065,#5066,#5067,#5068,#5069,
#5070,#5071,#5072,#5073,#5074,#5075,#5076,#5077,#5078,#5079,#5080,#5081,
#5082,#5083,#5084,#5085,#5086,#5087,#5088,#5089,#5090,#5091,#5092,#5093),
(#5094,#5095,#5096,#5097,#5098,#5099,#5100,#5101,#5102,#5103,#5104,#5105,
#5106,#5107,#5108,#5109,#5110,#5111,#5112,#5113,#5114,#5115,#5116,#5117,
#5118,#5119,#5120,#5121,#5122,#5123,#5124,#5125,#5126,#5127,#5128,#5129,
#5130,#5131,#5132,#5133,#5134,#5135,#5136,#5137,#5138,#5139,#5140,#5141,
#5142,#5143,#5144,#5145,#5146,#5147,#5148,#5149,#5150,#5151,#5152,#5153,
#5154,#5155,#5156,#5157,#5158,#5159,#5160,#5161,#5162,#5163,#5164,#5165,
#5166,#5167,#5168,#5169,#5170,#5171,#5172,#5173,#5174,#5175,#5176,#5177,
#5178,#5179,#5180,#5181,#5182,#5183,#5184,#5185,#5186,#5187,#5188,#5189,
#5190,#5191,#5192,#5193,#5194,#5195,#5196,#5197),(#5198,#5199,#5200,#5201,
#5202,#5203,#5204,#5205,#5206,#5207,#5208,#5209,#5210,#5211,#5212,#5213,
#5214,#5215,#5216,#5217,#5218,#5219,#5220,#5221,#5222,#5223,#5224,#5225,
#5226,#5227,#5228,#5229,#5230,#5231,#5232,#5233,#5234,#5235,#5236,#5237,
#5238,#5239,#5240,#5241,#5242,#5243,#5244,#5245,#5246,#5247,#5248,#5249,
#5250,#5251,#5252,#5253,#5254,#5255,#5256,#5257,#5258,#5259,#5260,#5261,
#5262,#5263,#5264,#5265,#5266,#5267,#5268,#5269,#5270,#5271,#5272,#5273,
#5274,#5275,#5276,#5277,#5278,#5279,#5280,#5281,#5282,#5283,#5284,#5285,
#5286,#5287,#5288,#5289,#5290,#5291,#5292,#5293,#5294,#5295,#5296,#5297,
#5298,#5299,#5300,#5301),(#5302,#5303,#5304,#5305,#5306,#5307,#5308,#5309,
#5310,#5311,#5312,#5313,#5314,#5315,#5316,#5317,#5318,#5319,#5320,#5321,
#5322,#5323,#5324,#5325,#5326,#5327,#5328,#5329,#5330,#5331,#5332,#5333,
#5334,#5335,#5336,#5337,#5338,#5339,#5340,#5341,#5342,#5343,#5344,#5345,
#5346,#5347,#5348,#5349,#5350,#5351,#5352,#5353,#5354,#5355,#5356,#5357,
#5358,#5359,#5360,#5361,#5362,#5363,#5364,#5365,#5366,#5367,#5368,#5369,
#5370,#5371,#5372,#5373,#5374,#5375,#5376,#5377,#5378,#5379,#5380,#5381,
#5382,#5383,#5384,#5385,#5386,#5387,#5388,#5389,#5390,#5391,#5392,#5393,
#5394,#5395,#5396,#5397,#5398,#5399,#5400,#5401,#5402,#5403,#5404,#5405),
(#5406,#5407,#5408,#5409,#5410,#5411,#5412,#5413,#5414,#5415,#5416,#5417,
#5418,#5419,#5420,#5421,#5422,#5423,#5424,#5425,#5426,#5427,#5428,#5429,
#5430,#5431,#5432,#5433,#5434,#5435,#5436,#5437,#5438,#5439,#5440,#5441,
#5442,#5443,#5444,#5445,#5446,#5447,#5448,#5449,#5450,#5451,#5452,#5453,
#5454,#5455,#5456,#5457,#5458,#5459,#5460,#5461,#5462,#5463,#5464,#5465,
#5466,#5467,#5468,#5469,#5470,#5471,#5472,#5473,#5474,#5475,#5476,#5477,
#5478,#5479,#5480,#5481,#5482,#5483,#5484,#5485,#5486,#5487,#5488,#5489,
#5490,#5491,#5492,#5493,#5494,#5495,#5496,#5497,#5498,#5499,#5500,#5501,
#5502,#5503,#5504,#5505,#5506,#5507,#5508,#5509),(#5510,#5511,#5512,#5513,
#5514,#5515,#5516,#5517,#5518,#5519,#5520,#5521,#5522,#5523,#5524,#5525,
#5526,#5527,#5528,#5529,#5530,#5531,#5532,#5533,#5534,#5535,#5536,#5537,
#5538,#5539,#5540,#5541,#5542,#5543,#5544,#5545,#5546,#5547,#5548,#5549,
#5550,#5551,#5552,#5553,#5554,#5555,#5556,#5557,#5558,#5559,#5560,#5561,
#5562,#5563,#5564,#5565,#5566,#5567,#5568,#5569,#5570,#5571,#5572,#5573,
#5574,#5575,#5576,#5577,#5578,#5579,#5580,#5581,#5582,#5583,#5584,#5585,
#5586,#5587,#5588,#5589,#5590,#5591,#5592,#5593,#5594,#5595,#5596,#5597,
#5598,#5599,#5600,#5601,#5602,#5603,#5604,#5605,#5606,#5607,#5608,#5609,
#5610,#5611,#5612,#5613),(#5614,#5615,#5616,#5617,#5618,#5619,#5620,#5621,
#5622,#5623,#5624,#5625,#5626,#5627,#5628,#5629,#5630,#5631,#5632,#5633,
#5634,#5635,#5636,#5637,#5638,#5639,#5640,#5641,#5642,#5643,#5644,#5645,
#5646,#5647,#5648,#5649,#5650,#5651,#5652,#5653,#5654,#5655,#5656,#5657,
#5658,#5659,#5660,#5661,#5662,#5663,#5664,#5665,#5666,#5667,#5668,#5669,
#5670,#5671,#5672,#5673,#5674,#5675,#5676,#5677,#5678,#5679,#5680,#5681,
#5682,#5683,#5684,#5685,#5686,#5687,#5688,#5689,#5690,#5691,#5692,#5693,
#5694,#5695,#5696,#5697,#5698,#5699,#5700,#5701,#5702,#5703,#5704,#5705,
#5706,#5707,#5708,#5709,#5710,#5711,#5712,#5713,#5714,#5715,#5716,#5717)),
 .UNSPECIFIED.,.T.,.F.,.F.)
B_SPLINE_SURFACE_WITH_KNOTS((4,3,3,4),(4,2,2,2,2,2,2,2,2,2,2,2,2,2,2,2,
2,2,2,2,2,2,2,2,2,2,2,2,2,2,2,2,2,2,2,2,2,2,2,2,2,2,2,2,2,2,2,2,2,2,2,4),
(0.499980401958503,0.5,1.,1.4999804019585),(0.,0.0155213821795324,0.0465641465385971,
0.0776069108976618,0.108649675256726,0.139692439615791,0.170735203974856,
0.201777968333921,0.232820732692985,0.26386349705205,0.294906261411162,
0.325949025770274,0.356991790129291,0.388034554488308,0.419077318847373,
0.450120083206437,0.46564146538597,0.481162847565502,0.496684229745034,
0.512205611924566,0.527726994104099,0.543248376283631,0.558769758463163,
0.574291140642696,0.589812522822228,0.605333905001761,0.620855287181293,
0.636376669360825,0.651898051540357,0.66741943371989,0.682940815899422,
0.698462198078954,0.713983580258487,0.729504962438019,0.745026344617551,
0.760547726797084,0.776069108976616,0.791590491156148,0.807111873335681,
0.822633255515213,0.838154637694745,0.853676019874278,0.86919740205381,
0.884718784233342,0.900240166412875,0.915761548592407,0.931282930771939,
0.946804312951471,0.973402156475736,0.986701078237868,0.993350539118934,
1.),.UNSPECIFIED.)
GEOMETRIC_REPRESENTATION_ITEM()
RATIONAL_B_SPLINE_SURFACE(((0.999921610906677,0.999921610906677,0.999921610906677,
0.999921610906677,0.999921610906677,0.999921610906677,0.999921610906677,
0.999921610906677,0.999921610906677,0.999921610906677,0.999921610906677,
0.999921610906677,0.999921610906677,0.999921610906677,0.999921610906677,
0.999921610906677,0.999921610906677,0.999921610906677,0.999921610906677,
0.999921610906677,0.999921610906677,0.999921610906677,0.999921610906677,
0.999921610906677,0.999921610906677,0.999921610906677,0.999921610906677,
0.999921610906677,0.999921610906677,0.999921610906677,0.999921610906677,
0.999921610906677,0.999921610906677,0.999921610906677,0.999921610906677,
0.999921610906677,0.999921610906677,0.999921610906677,0.999921610906677,
0.999921610906677,0.999921610906677,0.999921610906677,0.999921610906677,
0.999921610906677,0.999921610906677,0.999921610906677,0.999921610906677,
0.999921610906677,0.999921610906677,0.999921610906677,0.999921610906677,
0.999921610906677,0.999921610906677,0.999921610906677,0.999921610906677,
0.999921610906677,0.999921610906677,0.999921610906677,0.999921610906677,
0.999921610906677,0.999921610906677,0.999921610906677,0.999921610906677,
0.999921610906677,0.999921610906677,0.999921610906677,0.999921610906677,
0.999921610906677,0.999921610906677,0.999921610906677,0.999921610906677,
0.999921610906677,0.999921610906677,0.999921610906677,0.999921610906677,
0.999921610906677,0.999921610906677,0.999921610906677,0.999921610906677,
0.999921610906677,0.999921610906677,0.999921610906677,0.999921610906677,
0.999921610906677,0.999921610906677,0.999921610906677,0.999921610906677,
0.999921610906677,0.999921610906677,0.999921610906677,0.999921610906677,
0.999921610906677,0.999921610906677,0.999921610906677,0.999921610906677,
0.999921610906677,0.999921610906677,0.999921610906677,0.999921610906677,
0.999921610906677,0.999921610906677,0.999921610906677,0.999921610906677,
0.999921610906677),(0.999947739580229,0.999947739580229,0.999947739580229,
0.999947739580229,0.999947739580229,0.999947739580229,0.999947739580229,
0.999947739580229,0.999947739580229,0.999947739580229,0.999947739580229,
0.999947739580229,0.999947739580229,0.999947739580229,0.999947739580229,
0.999947739580229,0.999947739580229,0.999947739580229,0.999947739580229,
0.999947739580229,0.999947739580229,0.999947739580229,0.999947739580229,
0.999947739580229,0.999947739580229,0.999947739580229,0.999947739580229,
0.999947739580229,0.999947739580229,0.999947739580229,0.999947739580229,
0.999947739580229,0.999947739580229,0.999947739580229,0.999947739580229,
0.999947739580229,0.999947739580229,0.999947739580229,0.999947739580229,
0.999947739580229,0.999947739580229,0.999947739580229,0.999947739580229,
0.999947739580229,0.999947739580229,0.999947739580229,0.999947739580229,
0.999947739580229,0.999947739580229,0.999947739580229,0.999947739580229,
0.999947739580229,0.999947739580229,0.999947739580229,0.999947739580229,
0.999947739580229,0.999947739580229,0.999947739580229,0.999947739580229,
0.999947739580229,0.999947739580229,0.999947739580229,0.999947739580229,
0.999947739580229,0.999947739580229,0.999947739580229,0.999947739580229,
0.999947739580229,0.999947739580229,0.999947739580229,0.999947739580229,
0.999947739580229,0.999947739580229,0.999947739580229,0.999947739580229,
0.999947739580229,0.999947739580229,0.999947739580229,0.999947739580229,
0.999947739580229,0.999947739580229,0.999947739580229,0.999947739580229,
0.999947739580229,0.999947739580229,0.999947739580229,0.999947739580229,
0.999947739580229,0.999947739580229,0.999947739580229,0.999947739580229,
0.999947739580229,0.999947739580229,0.999947739580229,0.999947739580229,
0.999947739580229,0.999947739580229,0.999947739580229,0.999947739580229,
0.999947739580229,0.999947739580229,0.999947739580229,0.999947739580229,
0.999947739580229),(0.999973869278004,0.999973869278004,0.999973869278004,
0.999973869278004,0.999973869278004,0.999973869278004,0.999973869278004,
0.999973869278004,0.999973869278004,0.999973869278004,0.999973869278004,
0.999973869278004,0.999973869278004,0.999973869278004,0.999973869278004,
0.999973869278004,0.999973869278004,0.999973869278004,0.999973869278004,
0.999973869278004,0.999973869278004,0.999973869278004,0.999973869278004,
0.999973869278004,0.999973869278004,0.999973869278004,0.999973869278004,
0.999973869278004,0.999973869278004,0.999973869278004,0.999973869278004,
0.999973869278004,0.999973869278004,0.999973869278004,0.999973869278004,
0.999973869278004,0.999973869278004,0.999973869278004,0.999973869278004,
0.999973869278004,0.999973869278004,0.999973869278004,0.999973869278004,
0.999973869278004,0.999973869278004,0.999973869278004,0.999973869278004,
0.999973869278004,0.999973869278004,0.999973869278004,0.999973869278004,
0.999973869278004,0.999973869278004,0.999973869278004,0.999973869278004,
0.999973869278004,0.999973869278004,0.999973869278004,0.999973869278004,
0.999973869278004,0.999973869278004,0.999973869278004,0.999973869278004,
0.999973869278004,0.999973869278004,0.999973869278004,0.999973869278004,
0.999973869278004,0.999973869278004,0.999973869278004,0.999973869278004,
0.999973869278004,0.999973869278004,0.999973869278004,0.999973869278004,
0.999973869278004,0.999973869278004,0.999973869278004,0.999973869278004,
0.999973869278004,0.999973869278004,0.999973869278004,0.999973869278004,
0.999973869278004,0.999973869278004,0.999973869278004,0.999973869278004,
0.999973869278004,0.999973869278004,0.999973869278004,0.999973869278004,
0.999973869278004,0.999973869278004,0.999973869278004,0.999973869278004,
0.999973869278004,0.999973869278004,0.999973869278004,0.999973869278004,
0.999973869278004,0.999973869278004,0.999973869278004,0.999973869278004,
0.999973869278004),(1.,1.,1.,1.,1.,1.,1.,1.,1.,1.,1.,1.,1.,1.,1.,1.,1.,
1.,1.,1.,1.,1.,1.,1.,1.,1.,1.,1.,1.,1.,1.,1.,1.,1.,1.,1.,1.,1.,1.,1.,1.,
1.,1.,1.,1.,1.,1.,1.,1.,1.,1.,1.,1.,1.,1.,1.,1.,1.,1.,1.,1.,1.,1.,1.,1.,
1.,1.,1.,1.,1.,1.,1.,1.,1.,1.,1.,1.,1.,1.,1.,1.,1.,1.,1.,1.,1.,1.,1.,1.,
1.,1.,1.,1.,1.,1.,1.,1.,1.,1.,1.,1.,1.,1.,1.),(0.333333333333333,0.333333333333333,
0.333333333333333,0.333333333333333,0.333333333333333,0.333333333333333,
0.333333333333333,0.333333333333333,0.333333333333333,0.333333333333333,
0.333333333333333,0.333333333333333,0.333333333333333,0.333333333333333,
0.333333333333333,0.333333333333333,0.333333333333333,0.333333333333333,
0.333333333333333,0.333333333333333,0.333333333333333,0.333333333333333,
0.333333333333333,0.333333333333333,0.333333333333333,0.333333333333333,
0.333333333333333,0.333333333333333,0.333333333333333,0.333333333333333,
0.333333333333333,0.333333333333333,0.333333333333333,0.333333333333333,
0.333333333333333,0.333333333333333,0.333333333333333,0.333333333333333,
0.333333333333333,0.333333333333333,0.333333333333333,0.333333333333333,
0.333333333333333,0.333333333333333,0.333333333333333,0.333333333333333,
0.333333333333333,0.333333333333333,0.333333333333333,0.333333333333333,
0.333333333333333,0.333333333333333,0.333333333333333,0.333333333333333,
0.333333333333333,0.333333333333333,0.333333333333333,0.333333333333333,
0.333333333333333,0.333333333333333,0.333333333333333,0.333333333333333,
0.333333333333333,0.333333333333333,0.333333333333333,0.333333333333333,
0.333333333333333,0.333333333333333,0.333333333333333,0.333333333333333,
0.333333333333333,0.333333333333333,0.333333333333333,0.333333333333333,
0.333333333333333,0.333333333333333,0.333333333333333,0.333333333333333,
0.333333333333333,0.333333333333333,0.333333333333333,0.333333333333333,
0.333333333333333,0.333333333333333,0.333333333333333,0.333333333333333,
0.333333333333333,0.333333333333333,0.333333333333333,0.333333333333333,
0.333333333333333,0.333333333333333,0.333333333333333,0.333333333333333,
0.333333333333333,0.333333333333333,0.333333333333333,0.333333333333333,
0.333333333333333,0.333333333333333,0.333333333333333,0.333333333333333,
0.333333333333333,0.333333333333333),(0.333333333333333,0.333333333333333,
0.333333333333333,0.333333333333333,0.333333333333333,0.333333333333333,
0.333333333333333,0.333333333333333,0.333333333333333,0.333333333333333,
0.333333333333333,0.333333333333333,0.333333333333333,0.333333333333333,
0.333333333333333,0.333333333333333,0.333333333333333,0.333333333333333,
0.333333333333333,0.333333333333333,0.333333333333333,0.333333333333333,
0.333333333333333,0.333333333333333,0.333333333333333,0.333333333333333,
0.333333333333333,0.333333333333333,0.333333333333333,0.333333333333333,
0.333333333333333,0.333333333333333,0.333333333333333,0.333333333333333,
0.333333333333333,0.333333333333333,0.333333333333333,0.333333333333333,
0.333333333333333,0.333333333333333,0.333333333333333,0.333333333333333,
0.333333333333333,0.333333333333333,0.333333333333333,0.333333333333333,
0.333333333333333,0.333333333333333,0.333333333333333,0.333333333333333,
0.333333333333333,0.333333333333333,0.333333333333333,0.333333333333333,
0.333333333333333,0.333333333333333,0.333333333333333,0.333333333333333,
0.333333333333333,0.333333333333333,0.333333333333333,0.333333333333333,
0.333333333333333,0.333333333333333,0.333333333333333,0.333333333333333,
0.333333333333333,0.333333333333333,0.333333333333333,0.333333333333333,
0.333333333333333,0.333333333333333,0.333333333333333,0.333333333333333,
0.333333333333333,0.333333333333333,0.333333333333333,0.333333333333333,
0.333333333333333,0.333333333333333,0.333333333333333,0.333333333333333,
0.333333333333333,0.333333333333333,0.333333333333333,0.333333333333333,
0.333333333333333,0.333333333333333,0.333333333333333,0.333333333333333,
0.333333333333333,0.333333333333333,0.333333333333333,0.333333333333333,
0.333333333333333,0.333333333333333,0.333333333333333,0.333333333333333,
0.333333333333333,0.333333333333333,0.333333333333333,0.333333333333333,
0.333333333333333,0.333333333333333),(1.,1.,1.,1.,1.,1.,1.,1.,1.,1.,1.,
1.,1.,1.,1.,1.,1.,1.,1.,1.,1.,1.,1.,1.,1.,1.,1.,1.,1.,1.,1.,1.,1.,1.,1.,
1.,1.,1.,1.,1.,1.,1.,1.,1.,1.,1.,1.,1.,1.,1.,1.,1.,1.,1.,1.,1.,1.,1.,1.,
1.,1.,1.,1.,1.,1.,1.,1.,1.,1.,1.,1.,1.,1.,1.,1.,1.,1.,1.,1.,1.,1.,1.,1.,
1.,1.,1.,1.,1.,1.,1.,1.,1.,1.,1.,1.,1.,1.,1.,1.,1.,1.,1.,1.,1.),(0.33335946405533,
0.33335946405533,0.33335946405533,0.33335946405533,0.33335946405533,0.33335946405533,
0.33335946405533,0.33335946405533,0.33335946405533,0.33335946405533,0.33335946405533,
0.33335946405533,0.33335946405533,0.33335946405533,0.33335946405533,0.33335946405533,
0.33335946405533,0.33335946405533,0.33335946405533,0.33335946405533,0.33335946405533,
0.33335946405533,0.33335946405533,0.33335946405533,0.33335946405533,0.33335946405533,
0.33335946405533,0.33335946405533,0.33335946405533,0.33335946405533,0.33335946405533,
0.33335946405533,0.33335946405533,0.33335946405533,0.33335946405533,0.33335946405533,
0.33335946405533,0.33335946405533,0.33335946405533,0.33335946405533,0.33335946405533,
0.33335946405533,0.33335946405533,0.33335946405533,0.33335946405533,0.33335946405533,
0.33335946405533,0.33335946405533,0.33335946405533,0.33335946405533,0.33335946405533,
0.33335946405533,0.33335946405533,0.33335946405533,0.33335946405533,0.33335946405533,
0.33335946405533,0.33335946405533,0.33335946405533,0.33335946405533,0.33335946405533,
0.33335946405533,0.33335946405533,0.33335946405533,0.33335946405533,0.33335946405533,
0.33335946405533,0.33335946405533,0.33335946405533,0.33335946405533,0.33335946405533,
0.33335946405533,0.33335946405533,0.33335946405533,0.33335946405533,0.33335946405533,
0.33335946405533,0.33335946405533,0.33335946405533,0.33335946405533,0.33335946405533,
0.33335946405533,0.33335946405533,0.33335946405533,0.33335946405533,0.33335946405533,
0.33335946405533,0.33335946405533,0.33335946405533,0.33335946405533,0.33335946405533,
0.33335946405533,0.33335946405533,0.33335946405533,0.33335946405533,0.33335946405533,
0.33335946405533,0.33335946405533,0.33335946405533,0.33335946405533,0.33335946405533,
0.33335946405533,0.33335946405533,0.33335946405533),(0.333333334357555,
0.333333334357555,0.333333334357555,0.333333334357555,0.333333334357555,
0.333333334357555,0.333333334357555,0.333333334357555,0.333333334357555,
0.333333334357555,0.333333334357555,0.333333334357555,0.333333334357555,
0.333333334357555,0.333333334357555,0.333333334357555,0.333333334357555,
0.333333334357555,0.333333334357555,0.333333334357555,0.333333334357555,
0.333333334357555,0.333333334357555,0.333333334357555,0.333333334357555,
0.333333334357555,0.333333334357555,0.333333334357555,0.333333334357555,
0.333333334357555,0.333333334357555,0.333333334357555,0.333333334357555,
0.333333334357555,0.333333334357555,0.333333334357555,0.333333334357555,
0.333333334357555,0.333333334357555,0.333333334357555,0.333333334357555,
0.333333334357555,0.333333334357555,0.333333334357555,0.333333334357555,
0.333333334357555,0.333333334357555,0.333333334357555,0.333333334357555,
0.333333334357555,0.333333334357555,0.333333334357555,0.333333334357555,
0.333333334357555,0.333333334357555,0.333333334357555,0.333333334357555,
0.333333334357555,0.333333334357555,0.333333334357555,0.333333334357555,
0.333333334357555,0.333333334357555,0.333333334357555,0.333333334357555,
0.333333334357555,0.333333334357555,0.333333334357555,0.333333334357555,
0.333333334357555,0.333333334357555,0.333333334357555,0.333333334357555,
0.333333334357555,0.333333334357555,0.333333334357555,0.333333334357555,
0.333333334357555,0.333333334357555,0.333333334357555,0.333333334357555,
0.333333334357555,0.333333334357555,0.333333334357555,0.333333334357555,
0.333333334357555,0.333333334357555,0.333333334357555,0.333333334357555,
0.333333334357555,0.333333334357555,0.333333334357555,0.333333334357555,
0.333333334357555,0.333333334357555,0.333333334357555,0.333333334357555,
0.333333334357555,0.333333334357555,0.333333334357555,0.333333334357555,
0.333333334357555,0.333333334357555,0.333333334357555),(0.999921610906677,
0.999921610906677,0.999921610906677,0.999921610906677,0.999921610906677,
0.999921610906677,0.999921610906677,0.999921610906677,0.999921610906677,
0.999921610906677,0.999921610906677,0.999921610906677,0.999921610906677,
0.999921610906677,0.999921610906677,0.999921610906677,0.999921610906677,
0.999921610906677,0.999921610906677,0.999921610906677,0.999921610906677,
0.999921610906677,0.999921610906677,0.999921610906677,0.999921610906677,
0.999921610906677,0.999921610906677,0.999921610906677,0.999921610906677,
0.999921610906677,0.999921610906677,0.999921610906677,0.999921610906677,
0.999921610906677,0.999921610906677,0.999921610906677,0.999921610906677,
0.999921610906677,0.999921610906677,0.999921610906677,0.999921610906677,
0.999921610906677,0.999921610906677,0.999921610906677,0.999921610906677,
0.999921610906677,0.999921610906677,0.999921610906677,0.999921610906677,
0.999921610906677,0.999921610906677,0.999921610906677,0.999921610906677,
0.999921610906677,0.999921610906677,0.999921610906677,0.999921610906677,
0.999921610906677,0.999921610906677,0.999921610906677,0.999921610906677,
0.999921610906677,0.999921610906677,0.999921610906677,0.999921610906677,
0.999921610906677,0.999921610906677,0.999921610906677,0.999921610906677,
0.999921610906677,0.999921610906677,0.999921610906677,0.999921610906677,
0.999921610906677,0.999921610906677,0.999921610906677,0.999921610906677,
0.999921610906677,0.999921610906677,0.999921610906677,0.999921610906677,
0.999921610906677,0.999921610906677,0.999921610906677,0.999921610906677,
0.999921610906677,0.999921610906677,0.999921610906677,0.999921610906677,
0.999921610906677,0.999921610906677,0.999921610906677,0.999921610906677,
0.999921610906677,0.999921610906677,0.999921610906677,0.999921610906677,
0.999921610906677,0.999921610906677,0.999921610906677,0.999921610906677,
0.999921610906677,0.999921610906677,0.999921610906677)))
REPRESENTATION_ITEM('')
SURFACE()
);
#63=CONICAL_SURFACE('',#1021,1.61,0.785398163397466);
#64=SHAPE_REPRESENTATION_RELATIONSHIP('SRR','None',#5975,#71);
#65=SHAPE_REPRESENTATION_RELATIONSHIP('SRR','None',#5976,#72);
#66=SHAPE_REPRESENTATION_RELATIONSHIP('SRR','None',#5977,#73);
#67=SHAPE_REPRESENTATION_RELATIONSHIP('SRR','None',#5978,#74);
#68=SHAPE_REPRESENTATION_RELATIONSHIP('SRR','None',#5979,#75);
#69=SHAPE_REPRESENTATION_RELATIONSHIP('SRR','None',#5980,#76);
#70=SHAPE_REPRESENTATION_RELATIONSHIP('SRR','None',#5981,#77);
#71=ADVANCED_BREP_SHAPE_REPRESENTATION('',(#85),#5935);
#72=ADVANCED_BREP_SHAPE_REPRESENTATION('',(#86),#5936);
#73=ADVANCED_BREP_SHAPE_REPRESENTATION('',(#87),#5937);
#74=ADVANCED_BREP_SHAPE_REPRESENTATION('',(#88),#5938);
#75=ADVANCED_BREP_SHAPE_REPRESENTATION('',(#89),#5939);
#76=ADVANCED_BREP_SHAPE_REPRESENTATION('',(#90),#5940);
#77=ADVANCED_BREP_SHAPE_REPRESENTATION('',(#91),#5941);
#78=STYLED_ITEM('',(#6019),#85);
#79=STYLED_ITEM('',(#6020),#86);
#80=STYLED_ITEM('',(#6021),#87);
#81=STYLED_ITEM('',(#6022),#88);
#82=STYLED_ITEM('',(#6022),#89);
#83=STYLED_ITEM('',(#6020),#90);
#84=STYLED_ITEM('',(#6023),#91);
#85=MANIFOLD_SOLID_BREP('Body1',#925);
#86=MANIFOLD_SOLID_BREP('Body1',#926);
#87=MANIFOLD_SOLID_BREP('Body1',#927);
#88=MANIFOLD_SOLID_BREP('Body1',#928);
#89=MANIFOLD_SOLID_BREP('Body1',#929);
#90=MANIFOLD_SOLID_BREP('Body1',#930);
#91=MANIFOLD_SOLID_BREP('Body1',#931);
#92=FACE_BOUND('',#197,.T.);
#93=FACE_BOUND('',#199,.T.);
#94=FACE_BOUND('',#217,.T.);
#95=FACE_BOUND('',#219,.T.);
#96=FACE_BOUND('',#233,.T.);
#97=FACE_BOUND('',#242,.T.);
#98=FACE_BOUND('',#247,.T.);
#99=FACE_BOUND('',#249,.T.);
#100=PLANE('',#1018);
#101=PLANE('',#1019);
#102=PLANE('',#1027);
#103=PLANE('',#1028);
#104=PLANE('',#1037);
#105=PLANE('',#1039);
#106=PLANE('',#1051);
#107=PLANE('',#1052);
#108=PLANE('',#1053);
#109=PLANE('',#1054);
#110=PLANE('',#1055);
#111=PLANE('',#1056);
#112=PLANE('',#1057);
#113=PLANE('',#1058);
#114=PLANE('',#1059);
#115=PLANE('',#1060);
#116=PLANE('',#1061);
#117=PLANE('',#1062);
#118=PLANE('',#1063);
#119=PLANE('',#1064);
#120=PLANE('',#1065);
#121=PLANE('',#1066);
#122=PLANE('',#1071);
#123=PLANE('',#1072);
#124=PLANE('',#1073);
#125=PLANE('',#1074);
#126=PLANE('',#1075);
#127=PLANE('',#1076);
#128=PLANE('',#1077);
#129=PLANE('',#1085);
#130=PLANE('',#1086);
#131=PLANE('',#1087);
#132=PLANE('',#1092);
#133=PLANE('',#1093);
#134=PLANE('',#1094);
#135=PLANE('',#1095);
#136=PLANE('',#1096);
#137=PLANE('',#1097);
#138=PLANE('',#1098);
#139=PLANE('',#1099);
#140=FACE_OUTER_BOUND('',#194,.T.);
#141=FACE_OUTER_BOUND('',#195,.T.);
#142=FACE_OUTER_BOUND('',#196,.T.);
#143=FACE_OUTER_BOUND('',#198,.T.);
#144=FACE_OUTER_BOUND('',#200,.T.);
#145=FACE_OUTER_BOUND('',#201,.T.);
#146=FACE_OUTER_BOUND('',#202,.T.);
#147=FACE_OUTER_BOUND('',#203,.T.);
#148=FACE_OUTER_BOUND('',#204,.T.);
#149=FACE_OUTER_BOUND('',#205,.T.);
#150=FACE_OUTER_BOUND('',#206,.T.);
#151=FACE_OUTER_BOUND('',#207,.T.);
#152=FACE_OUTER_BOUND('',#208,.T.);
#153=FACE_OUTER_BOUND('',#209,.T.);
#154=FACE_OUTER_BOUND('',#210,.T.);
#155=FACE_OUTER_BOUND('',#211,.T.);
#156=FACE_OUTER_BOUND('',#212,.T.);
#157=FACE_OUTER_BOUND('',#213,.T.);
#158=FACE_OUTER_BOUND('',#214,.T.);
#159=FACE_OUTER_BOUND('',#215,.T.);
#160=FACE_OUTER_BOUND('',#216,.T.);
#161=FACE_OUTER_BOUND('',#218,.T.);
#162=FACE_OUTER_BOUND('',#220,.T.);
#163=FACE_OUTER_BOUND('',#221,.T.);
#164=FACE_OUTER_BOUND('',#222,.T.);
#165=FACE_OUTER_BOUND('',#223,.T.);
#166=FACE_OUTER_BOUND('',#224,.T.);
#167=FACE_OUTER_BOUND('',#225,.T.);
#168=FACE_OUTER_BOUND('',#226,.T.);
#169=FACE_OUTER_BOUND('',#227,.T.);
#170=FACE_OUTER_BOUND('',#228,.T.);
#171=FACE_OUTER_BOUND('',#229,.T.);
#172=FACE_OUTER_BOUND('',#230,.T.);
#173=FACE_OUTER_BOUND('',#231,.T.);
#174=FACE_OUTER_BOUND('',#232,.T.);
#175=FACE_OUTER_BOUND('',#234,.T.);
#176=FACE_OUTER_BOUND('',#235,.T.);
#177=FACE_OUTER_BOUND('',#236,.T.);
#178=FACE_OUTER_BOUND('',#237,.T.);
#179=FACE_OUTER_BOUND('',#238,.T.);
#180=FACE_OUTER_BOUND('',#239,.T.);
#181=FACE_OUTER_BOUND('',#240,.T.);
#182=FACE_OUTER_BOUND('',#241,.T.);
#183=FACE_OUTER_BOUND('',#243,.T.);
#184=FACE_OUTER_BOUND('',#244,.T.);
#185=FACE_OUTER_BOUND('',#245,.T.);
#186=FACE_OUTER_BOUND('',#246,.T.);
#187=FACE_OUTER_BOUND('',#248,.T.);
#188=FACE_OUTER_BOUND('',#250,.T.);
#189=FACE_OUTER_BOUND('',#251,.T.);
#190=FACE_OUTER_BOUND('',#252,.T.);
#191=FACE_OUTER_BOUND('',#253,.T.);
#192=FACE_OUTER_BOUND('',#254,.T.);
#193=FACE_OUTER_BOUND('',#255,.T.);
#194=EDGE_LOOP('',(#634,#635,#636,#637));
#195=EDGE_LOOP('',(#638,#639,#640,#641));
#196=EDGE_LOOP('',(#642));
#197=EDGE_LOOP('',(#643));
#198=EDGE_LOOP('',(#644));
#199=EDGE_LOOP('',(#645));
#200=EDGE_LOOP('',(#646,#647,#648,#649,#650));
#201=EDGE_LOOP('',(#651,#652,#653,#654,#655));
#202=EDGE_LOOP('',(#656));
#203=EDGE_LOOP('',(#657));
#204=EDGE_LOOP('',(#658,#659,#660,#661,#662));
#205=EDGE_LOOP('',(#663,#664,#665,#666,#667));
#206=EDGE_LOOP('',(#668,#669,#670,#671,#672));
#207=EDGE_LOOP('',(#673,#674));
#208=EDGE_LOOP('',(#675,#676,#677,#678,#679));
#209=EDGE_LOOP('',(#680,#681));
#210=EDGE_LOOP('',(#682,#683,#684,#685));
#211=EDGE_LOOP('',(#686,#687,#688,#689,#690,#691,#692,#693,#694,#695,#696,
#697));
#212=EDGE_LOOP('',(#698,#699,#700,#701));
#213=EDGE_LOOP('',(#702,#703,#704,#705));
#214=EDGE_LOOP('',(#706,#707,#708));
#215=EDGE_LOOP('',(#709,#710,#711));
#216=EDGE_LOOP('',(#712,#713,#714,#715,#716,#717,#718,#719,#720,#721,#722,
#723));
#217=EDGE_LOOP('',(#724));
#218=EDGE_LOOP('',(#725,#726,#727,#728,#729,#730,#731,#732,#733,#734,#735,
#736,#737,#738));
#219=EDGE_LOOP('',(#739));
#220=EDGE_LOOP('',(#740,#741,#742,#743,#744));
#221=EDGE_LOOP('',(#745,#746,#747,#748));
#222=EDGE_LOOP('',(#749,#750,#751,#752));
#223=EDGE_LOOP('',(#753,#754,#755,#756));
#224=EDGE_LOOP('',(#757,#758,#759,#760));
#225=EDGE_LOOP('',(#761,#762,#763,#764,#765));
#226=EDGE_LOOP('',(#766,#767,#768,#769,#770,#771));
#227=EDGE_LOOP('',(#772,#773));
#228=EDGE_LOOP('',(#774));
#229=EDGE_LOOP('',(#775,#776,#777));
#230=EDGE_LOOP('',(#778,#779,#780,#781));
#231=EDGE_LOOP('',(#782));
#232=EDGE_LOOP('',(#783));
#233=EDGE_LOOP('',(#784,#785,#786,#787));
#234=EDGE_LOOP('',(#788,#789,#790,#791));
#235=EDGE_LOOP('',(#792,#793,#794,#795));
#236=EDGE_LOOP('',(#796,#797,#798,#799));
#237=EDGE_LOOP('',(#800,#801,#802,#803));
#238=EDGE_LOOP('',(#804,#805,#806,#807));
#239=EDGE_LOOP('',(#808,#809,#810,#811));
#240=EDGE_LOOP('',(#812,#813,#814,#815));
#241=EDGE_LOOP('',(#816));
#242=EDGE_LOOP('',(#817));
#243=EDGE_LOOP('',(#818));
#244=EDGE_LOOP('',(#819));
#245=EDGE_LOOP('',(#820,#821,#822,#823));
#246=EDGE_LOOP('',(#824,#825,#826,#827,#828,#829));
#247=EDGE_LOOP('',(#830));
#248=EDGE_LOOP('',(#831,#832,#833,#834,#835,#836));
#249=EDGE_LOOP('',(#837));
#250=EDGE_LOOP('',(#838,#839,#840,#841));
#251=EDGE_LOOP('',(#842,#843,#844,#845));
#252=EDGE_LOOP('',(#846,#847,#848,#849));
#253=EDGE_LOOP('',(#850,#851,#852,#853));
#254=EDGE_LOOP('',(#854,#855,#856,#857));
#255=EDGE_LOOP('',(#858,#859,#860,#861));
#256=LINE('',#1397,#334);
#257=LINE('',#1403,#335);
#258=LINE('',#1414,#336);
#259=LINE('',#1418,#337);
#260=LINE('',#5725,#338);
#261=LINE('',#5731,#339);
#262=LINE('',#5735,#340);
#263=LINE('',#5739,#341);
#264=LINE('',#5743,#342);
#265=LINE('',#5747,#343);
#266=LINE('',#5751,#344);
#267=LINE('',#5753,#345);
#268=LINE('',#5754,#346);
#269=LINE('',#5758,#347);
#270=LINE('',#5760,#348);
#271=LINE('',#5762,#349);
#272=LINE('',#5763,#350);
#273=LINE('',#5767,#351);
#274=LINE('',#5769,#352);
#275=LINE('',#5770,#353);
#276=LINE('',#5774,#354);
#277=LINE('',#5776,#355);
#278=LINE('',#5777,#356);
#279=LINE('',#5779,#357);
#280=LINE('',#5781,#358);
#281=LINE('',#5783,#359);
#282=LINE('',#5784,#360);
#283=LINE('',#5786,#361);
#284=LINE('',#5788,#362);
#285=LINE('',#5790,#363);
#286=LINE('',#5791,#364);
#287=LINE('',#5793,#365);
#288=LINE('',#5795,#366);
#289=LINE('',#5796,#367);
#290=LINE('',#5797,#368);
#291=LINE('',#5798,#369);
#292=LINE('',#5800,#370);
#293=LINE('',#5802,#371);
#294=LINE('',#5803,#372);
#295=LINE('',#5805,#373);
#296=LINE('',#5806,#374);
#297=LINE('',#5808,#375);
#298=LINE('',#5810,#376);
#299=LINE('',#5814,#377);
#300=LINE('',#5824,#378);
#301=LINE('',#5830,#379);
#302=LINE('',#5832,#380);
#303=LINE('',#5834,#381);
#304=LINE('',#5835,#382);
#305=LINE('',#5838,#383);
#306=LINE('',#5840,#384);
#307=LINE('',#5841,#385);
#308=LINE('',#5844,#386);
#309=LINE('',#5845,#387);
#310=LINE('',#5848,#388);
#311=LINE('',#5849,#389);
#312=LINE('',#5851,#390);
#313=LINE('',#5858,#391);
#314=LINE('',#5864,#392);
#315=LINE('',#5874,#393);
#316=LINE('',#5879,#394);
#317=LINE('',#5881,#395);
#318=LINE('',#5883,#396);
#319=LINE('',#5885,#397);
#320=LINE('',#5887,#398);
#321=LINE('',#5888,#399);
#322=LINE('',#5892,#400);
#323=LINE('',#5894,#401);
#324=LINE('',#5896,#402);
#325=LINE('',#5898,#403);
#326=LINE('',#5900,#404);
#327=LINE('',#5901,#405);
#328=LINE('',#5903,#406);
#329=LINE('',#5904,#407);
#330=LINE('',#5906,#408);
#331=LINE('',#5908,#409);
#332=LINE('',#5910,#410);
#333=LINE('',#5912,#411);
#334=VECTOR('',#1119,2.);
#335=VECTOR('',#1126,2.5);
#336=VECTOR('',#1141,1.61);
#337=VECTOR('',#1146,2.);
#338=VECTOR('',#1181,2.65);
#339=VECTOR('',#1188,2.5);
#340=VECTOR('',#1191,1000.);
#341=VECTOR('',#1194,1000.);
#342=VECTOR('',#1197,1000.);
#343=VECTOR('',#1200,1000.);
#344=VECTOR('',#1205,1000.);
#345=VECTOR('',#1206,1000.);
#346=VECTOR('',#1207,1000.);
#347=VECTOR('',#1210,1000.);
#348=VECTOR('',#1211,1000.);
#349=VECTOR('',#1212,1000.);
#350=VECTOR('',#1213,1000.);
#351=VECTOR('',#1216,1000.);
#352=VECTOR('',#1217,1000.);
#353=VECTOR('',#1218,1000.);
#354=VECTOR('',#1221,1000.);
#355=VECTOR('',#1222,1000.);
#356=VECTOR('',#1223,1000.);
#357=VECTOR('',#1226,1000.);
#358=VECTOR('',#1227,1000.);
#359=VECTOR('',#1228,1000.);
#360=VECTOR('',#1229,1000.);
#361=VECTOR('',#1230,1000.);
#362=VECTOR('',#1231,1000.);
#363=VECTOR('',#1232,1000.);
#364=VECTOR('',#1233,1000.);
#365=VECTOR('',#1236,1000.);
#366=VECTOR('',#1237,1000.);
#367=VECTOR('',#1238,1000.);
#368=VECTOR('',#1239,1000.);
#369=VECTOR('',#1240,1000.);
#370=VECTOR('',#1241,1000.);
#371=VECTOR('',#1242,1000.);
#372=VECTOR('',#1243,1000.);
#373=VECTOR('',#1246,1000.);
#374=VECTOR('',#1247,1000.);
#375=VECTOR('',#1250,1000.);
#376=VECTOR('',#1253,1000.);
#377=VECTOR('',#1260,1000.);
#378=VECTOR('',#1275,6.);
#379=VECTOR('',#1282,1000.);
#380=VECTOR('',#1283,1000.);
#381=VECTOR('',#1284,1000.);
#382=VECTOR('',#1285,1000.);
#383=VECTOR('',#1288,1000.);
#384=VECTOR('',#1289,1000.);
#385=VECTOR('',#1290,1000.);
#386=VECTOR('',#1293,1000.);
#387=VECTOR('',#1294,1000.);
#388=VECTOR('',#1297,1000.);
#389=VECTOR('',#1298,1000.);
#390=VECTOR('',#1301,1000.);
#391=VECTOR('',#1310,6.);
#392=VECTOR('',#1317,7.);
#393=VECTOR('',#1332,2.);
#394=VECTOR('',#1337,1000.);
#395=VECTOR('',#1338,1000.);
#396=VECTOR('',#1339,1000.);
#397=VECTOR('',#1340,1000.);
#398=VECTOR('',#1341,1000.);
#399=VECTOR('',#1342,1000.);
#400=VECTOR('',#1345,1000.);
#401=VECTOR('',#1346,1000.);
#402=VECTOR('',#1347,1000.);
#403=VECTOR('',#1348,1000.);
#404=VECTOR('',#1349,1000.);
#405=VECTOR('',#1350,1000.);
#406=VECTOR('',#1353,1000.);
#407=VECTOR('',#1354,1000.);
#408=VECTOR('',#1357,1000.);
#409=VECTOR('',#1360,1000.);
#410=VECTOR('',#1363,1000.);
#411=VECTOR('',#1366,1000.);
#412=CIRCLE('',#1013,2.);
#413=CIRCLE('',#1014,2.);
#414=CIRCLE('',#1016,2.5);
#415=CIRCLE('',#1017,2.5);
#416=CIRCLE('',#1022,2.);
#417=CIRCLE('',#1023,2.);
#418=CIRCLE('',#1024,1.61);
#419=CIRCLE('',#1026,2.);
#420=CIRCLE('',#1030,0.5);
#421=CIRCLE('',#1031,0.5);
#422=CIRCLE('',#1032,0.5);
#423=CIRCLE('',#1033,0.5);
#424=CIRCLE('',#1034,0.5);
#425=CIRCLE('',#1035,0.5);
#426=CIRCLE('',#1036,0.5);
#427=CIRCLE('',#1038,0.5);
#428=CIRCLE('',#1042,2.65);
#429=CIRCLE('',#1043,2.65);
#430=CIRCLE('',#1045,2.5);
#431=CIRCLE('',#1046,2.5);
#432=CIRCLE('',#1047,2.5);
#433=CIRCLE('',#1048,2.5);
#434=CIRCLE('',#1049,2.5);
#435=CIRCLE('',#1050,2.5);
#436=CIRCLE('',#1069,6.);
#437=CIRCLE('',#1070,6.);
#438=CIRCLE('',#1080,6.);
#439=CIRCLE('',#1081,6.);
#440=CIRCLE('',#1083,7.);
#441=CIRCLE('',#1084,7.);
#442=CIRCLE('',#1090,2.);
#443=CIRCLE('',#1091,2.);
#444=VERTEX_POINT('',#1394);
#445=VERTEX_POINT('',#1396);
#446=VERTEX_POINT('',#1400);
#447=VERTEX_POINT('',#1402);
#448=VERTEX_POINT('',#1409);
#449=VERTEX_POINT('',#1410);
#450=VERTEX_POINT('',#1413);
#451=VERTEX_POINT('',#1417);
#452=VERTEX_POINT('',#2151);
#453=VERTEX_POINT('',#2152);
#454=VERTEX_POINT('',#2154);
#455=VERTEX_POINT('',#2309);
#456=VERTEX_POINT('',#2311);
#457=VERTEX_POINT('',#3374);
#458=VERTEX_POINT('',#3375);
#459=VERTEX_POINT('',#3377);
#460=VERTEX_POINT('',#5722);
#461=VERTEX_POINT('',#5724);
#462=VERTEX_POINT('',#5728);
#463=VERTEX_POINT('',#5730);
#464=VERTEX_POINT('',#5732);
#465=VERTEX_POINT('',#5734);
#466=VERTEX_POINT('',#5736);
#467=VERTEX_POINT('',#5738);
#468=VERTEX_POINT('',#5740);
#469=VERTEX_POINT('',#5742);
#470=VERTEX_POINT('',#5744);
#471=VERTEX_POINT('',#5746);
#472=VERTEX_POINT('',#5750);
#473=VERTEX_POINT('',#5752);
#474=VERTEX_POINT('',#5756);
#475=VERTEX_POINT('',#5757);
#476=VERTEX_POINT('',#5759);
#477=VERTEX_POINT('',#5761);
#478=VERTEX_POINT('',#5765);
#479=VERTEX_POINT('',#5766);
#480=VERTEX_POINT('',#5768);
#481=VERTEX_POINT('',#5772);
#482=VERTEX_POINT('',#5773);
#483=VERTEX_POINT('',#5775);
#484=VERTEX_POINT('',#5780);
#485=VERTEX_POINT('',#5782);
#486=VERTEX_POINT('',#5785);
#487=VERTEX_POINT('',#5787);
#488=VERTEX_POINT('',#5789);
#489=VERTEX_POINT('',#5794);
#490=VERTEX_POINT('',#5799);
#491=VERTEX_POINT('',#5801);
#492=VERTEX_POINT('',#5821);
#493=VERTEX_POINT('',#5823);
#494=VERTEX_POINT('',#5828);
#495=VERTEX_POINT('',#5829);
#496=VERTEX_POINT('',#5831);
#497=VERTEX_POINT('',#5833);
#498=VERTEX_POINT('',#5837);
#499=VERTEX_POINT('',#5839);
#500=VERTEX_POINT('',#5843);
#501=VERTEX_POINT('',#5847);
#502=VERTEX_POINT('',#5855);
#503=VERTEX_POINT('',#5857);
#504=VERTEX_POINT('',#5861);
#505=VERTEX_POINT('',#5863);
#506=VERTEX_POINT('',#5871);
#507=VERTEX_POINT('',#5873);
#508=VERTEX_POINT('',#5877);
#509=VERTEX_POINT('',#5878);
#510=VERTEX_POINT('',#5880);
#511=VERTEX_POINT('',#5882);
#512=VERTEX_POINT('',#5884);
#513=VERTEX_POINT('',#5886);
#514=VERTEX_POINT('',#5890);
#515=VERTEX_POINT('',#5891);
#516=VERTEX_POINT('',#5893);
#517=VERTEX_POINT('',#5895);
#518=VERTEX_POINT('',#5897);
#519=VERTEX_POINT('',#5899);
#520=EDGE_CURVE('',#444,#444,#412,.T.);
#521=EDGE_CURVE('',#444,#445,#256,.T.);
#522=EDGE_CURVE('',#445,#445,#413,.T.);
#523=EDGE_CURVE('',#446,#446,#414,.T.);
#524=EDGE_CURVE('',#446,#447,#257,.T.);
#525=EDGE_CURVE('',#447,#447,#415,.T.);
#526=EDGE_CURVE('',#448,#449,#416,.T.);
#527=EDGE_CURVE('',#449,#448,#417,.T.);
#528=EDGE_CURVE('',#449,#450,#258,.T.);
#529=EDGE_CURVE('',#450,#450,#418,.T.);
#530=EDGE_CURVE('',#448,#451,#259,.T.);
#531=EDGE_CURVE('',#451,#451,#419,.T.);
#532=EDGE_CURVE('',#452,#453,#420,.T.);
#533=EDGE_CURVE('',#453,#454,#55,.T.);
#534=EDGE_CURVE('',#454,#455,#421,.T.);
#535=EDGE_CURVE('',#455,#456,#422,.T.);
#536=EDGE_CURVE('',#452,#456,#56,.T.);
#537=EDGE_CURVE('',#457,#458,#423,.T.);
#538=EDGE_CURVE('',#458,#459,#57,.T.);
#539=EDGE_CURVE('',#456,#459,#424,.T.);
#540=EDGE_CURVE('',#457,#455,#58,.T.);
#541=EDGE_CURVE('',#458,#457,#425,.T.);
#542=EDGE_CURVE('',#459,#454,#426,.T.);
#543=EDGE_CURVE('',#453,#452,#427,.T.);
#544=EDGE_CURVE('',#460,#460,#428,.T.);
#545=EDGE_CURVE('',#460,#461,#260,.T.);
#546=EDGE_CURVE('',#461,#461,#429,.T.);
#547=EDGE_CURVE('',#462,#462,#430,.T.);
#548=EDGE_CURVE('',#462,#463,#261,.T.);
#549=EDGE_CURVE('',#463,#464,#431,.T.);
#550=EDGE_CURVE('',#464,#465,#262,.T.);
#551=EDGE_CURVE('',#465,#466,#432,.T.);
#552=EDGE_CURVE('',#467,#466,#263,.T.);
#553=EDGE_CURVE('',#467,#468,#433,.T.);
#554=EDGE_CURVE('',#469,#468,#264,.T.);
#555=EDGE_CURVE('',#469,#470,#434,.T.);
#556=EDGE_CURVE('',#470,#471,#265,.T.);
#557=EDGE_CURVE('',#471,#463,#435,.T.);
#558=EDGE_CURVE('',#465,#472,#266,.T.);
#559=EDGE_CURVE('',#472,#473,#267,.T.);
#560=EDGE_CURVE('',#466,#473,#268,.T.);
#561=EDGE_CURVE('',#474,#475,#269,.T.);
#562=EDGE_CURVE('',#475,#476,#270,.T.);
#563=EDGE_CURVE('',#477,#476,#271,.T.);
#564=EDGE_CURVE('',#477,#474,#272,.T.);
#565=EDGE_CURVE('',#478,#479,#273,.T.);
#566=EDGE_CURVE('',#478,#480,#274,.T.);
#567=EDGE_CURVE('',#480,#479,#275,.T.);
#568=EDGE_CURVE('',#481,#482,#276,.T.);
#569=EDGE_CURVE('',#481,#483,#277,.T.);
#570=EDGE_CURVE('',#482,#483,#278,.T.);
#571=EDGE_CURVE('',#467,#468,#279,.T.);
#572=EDGE_CURVE('',#473,#484,#280,.T.);
#573=EDGE_CURVE('',#484,#485,#281,.T.);
#574=EDGE_CURVE('',#485,#477,#282,.T.);
#575=EDGE_CURVE('',#476,#486,#283,.T.);
#576=EDGE_CURVE('',#486,#487,#284,.T.);
#577=EDGE_CURVE('',#487,#488,#285,.T.);
#578=EDGE_CURVE('',#488,#469,#286,.T.);
#579=EDGE_CURVE('',#464,#471,#287,.T.);
#580=EDGE_CURVE('',#489,#470,#288,.T.);
#581=EDGE_CURVE('',#482,#489,#289,.T.);
#582=EDGE_CURVE('',#483,#478,#290,.T.);
#583=EDGE_CURVE('',#479,#475,#291,.T.);
#584=EDGE_CURVE('',#490,#474,#292,.T.);
#585=EDGE_CURVE('',#491,#490,#293,.T.);
#586=EDGE_CURVE('',#472,#491,#294,.T.);
#587=EDGE_CURVE('',#487,#481,#295,.T.);
#588=EDGE_CURVE('',#489,#488,#296,.T.);
#589=EDGE_CURVE('',#490,#485,#297,.T.);
#590=EDGE_CURVE('',#491,#484,#298,.T.);
#591=EDGE_CURVE('',#480,#486,#299,.T.);
#592=EDGE_CURVE('',#492,#492,#436,.T.);
#593=EDGE_CURVE('',#492,#493,#300,.T.);
#594=EDGE_CURVE('',#493,#493,#437,.T.);
#595=EDGE_CURVE('',#494,#495,#301,.T.);
#596=EDGE_CURVE('',#494,#496,#302,.T.);
#597=EDGE_CURVE('',#496,#497,#303,.T.);
#598=EDGE_CURVE('',#497,#495,#304,.T.);
#599=EDGE_CURVE('',#494,#498,#305,.T.);
#600=EDGE_CURVE('',#499,#498,#306,.T.);
#601=EDGE_CURVE('',#496,#499,#307,.T.);
#602=EDGE_CURVE('',#500,#495,#308,.T.);
#603=EDGE_CURVE('',#498,#500,#309,.T.);
#604=EDGE_CURVE('',#499,#501,#310,.T.);
#605=EDGE_CURVE('',#501,#497,#311,.T.);
#606=EDGE_CURVE('',#501,#500,#312,.T.);
#607=EDGE_CURVE('',#502,#502,#438,.T.);
#608=EDGE_CURVE('',#502,#503,#313,.T.);
#609=EDGE_CURVE('',#503,#503,#439,.T.);
#610=EDGE_CURVE('',#504,#504,#440,.T.);
#611=EDGE_CURVE('',#504,#505,#314,.T.);
#612=EDGE_CURVE('',#505,#505,#441,.T.);
#613=EDGE_CURVE('',#506,#506,#442,.T.);
#614=EDGE_CURVE('',#506,#507,#315,.T.);
#615=EDGE_CURVE('',#507,#507,#443,.T.);
#616=EDGE_CURVE('',#508,#509,#316,.T.);
#617=EDGE_CURVE('',#509,#510,#317,.T.);
#618=EDGE_CURVE('',#510,#511,#318,.T.);
#619=EDGE_CURVE('',#511,#512,#319,.T.);
#620=EDGE_CURVE('',#512,#513,#320,.T.);
#621=EDGE_CURVE('',#513,#508,#321,.T.);
#622=EDGE_CURVE('',#514,#515,#322,.T.);
#623=EDGE_CURVE('',#516,#514,#323,.T.);
#624=EDGE_CURVE('',#517,#516,#324,.T.);
#625=EDGE_CURVE('',#518,#517,#325,.T.);
#626=EDGE_CURVE('',#519,#518,#326,.T.);
#627=EDGE_CURVE('',#515,#519,#327,.T.);
#628=EDGE_CURVE('',#509,#515,#328,.T.);
#629=EDGE_CURVE('',#508,#514,#329,.T.);
#630=EDGE_CURVE('',#510,#519,#330,.T.);
#631=EDGE_CURVE('',#511,#518,#331,.T.);
#632=EDGE_CURVE('',#512,#517,#332,.T.);
#633=EDGE_CURVE('',#513,#516,#333,.T.);
#634=ORIENTED_EDGE('',*,*,#520,.T.);
#635=ORIENTED_EDGE('',*,*,#521,.T.);
#636=ORIENTED_EDGE('',*,*,#522,.F.);
#637=ORIENTED_EDGE('',*,*,#521,.F.);
#638=ORIENTED_EDGE('',*,*,#523,.T.);
#639=ORIENTED_EDGE('',*,*,#524,.T.);
#640=ORIENTED_EDGE('',*,*,#525,.F.);
#641=ORIENTED_EDGE('',*,*,#524,.F.);
#642=ORIENTED_EDGE('',*,*,#525,.T.);
#643=ORIENTED_EDGE('',*,*,#520,.F.);
#644=ORIENTED_EDGE('',*,*,#523,.F.);
#645=ORIENTED_EDGE('',*,*,#522,.T.);
#646=ORIENTED_EDGE('',*,*,#526,.F.);
#647=ORIENTED_EDGE('',*,*,#527,.F.);
#648=ORIENTED_EDGE('',*,*,#528,.T.);
#649=ORIENTED_EDGE('',*,*,#529,.T.);
#650=ORIENTED_EDGE('',*,*,#528,.F.);
#651=ORIENTED_EDGE('',*,*,#526,.T.);
#652=ORIENTED_EDGE('',*,*,#527,.T.);
#653=ORIENTED_EDGE('',*,*,#530,.T.);
#654=ORIENTED_EDGE('',*,*,#531,.F.);
#655=ORIENTED_EDGE('',*,*,#530,.F.);
#656=ORIENTED_EDGE('',*,*,#531,.T.);
#657=ORIENTED_EDGE('',*,*,#529,.F.);
#658=ORIENTED_EDGE('',*,*,#532,.T.);
#659=ORIENTED_EDGE('',*,*,#533,.T.);
#660=ORIENTED_EDGE('',*,*,#534,.T.);
#661=ORIENTED_EDGE('',*,*,#535,.T.);
#662=ORIENTED_EDGE('',*,*,#536,.F.);
#663=ORIENTED_EDGE('',*,*,#537,.T.);
#664=ORIENTED_EDGE('',*,*,#538,.T.);
#665=ORIENTED_EDGE('',*,*,#539,.F.);
#666=ORIENTED_EDGE('',*,*,#535,.F.);
#667=ORIENTED_EDGE('',*,*,#540,.F.);
#668=ORIENTED_EDGE('',*,*,#538,.F.);
#669=ORIENTED_EDGE('',*,*,#541,.T.);
#670=ORIENTED_EDGE('',*,*,#540,.T.);
#671=ORIENTED_EDGE('',*,*,#534,.F.);
#672=ORIENTED_EDGE('',*,*,#542,.F.);
#673=ORIENTED_EDGE('',*,*,#537,.F.);
#674=ORIENTED_EDGE('',*,*,#541,.F.);
#675=ORIENTED_EDGE('',*,*,#533,.F.);
#676=ORIENTED_EDGE('',*,*,#543,.T.);
#677=ORIENTED_EDGE('',*,*,#536,.T.);
#678=ORIENTED_EDGE('',*,*,#539,.T.);
#679=ORIENTED_EDGE('',*,*,#542,.T.);
#680=ORIENTED_EDGE('',*,*,#532,.F.);
#681=ORIENTED_EDGE('',*,*,#543,.F.);
#682=ORIENTED_EDGE('',*,*,#544,.T.);
#683=ORIENTED_EDGE('',*,*,#545,.T.);
#684=ORIENTED_EDGE('',*,*,#546,.T.);
#685=ORIENTED_EDGE('',*,*,#545,.F.);
#686=ORIENTED_EDGE('',*,*,#547,.F.);
#687=ORIENTED_EDGE('',*,*,#548,.T.);
#688=ORIENTED_EDGE('',*,*,#549,.T.);
#689=ORIENTED_EDGE('',*,*,#550,.T.);
#690=ORIENTED_EDGE('',*,*,#551,.T.);
#691=ORIENTED_EDGE('',*,*,#552,.F.);
#692=ORIENTED_EDGE('',*,*,#553,.T.);
#693=ORIENTED_EDGE('',*,*,#554,.F.);
#694=ORIENTED_EDGE('',*,*,#555,.T.);
#695=ORIENTED_EDGE('',*,*,#556,.T.);
#696=ORIENTED_EDGE('',*,*,#557,.T.);
#697=ORIENTED_EDGE('',*,*,#548,.F.);
#698=ORIENTED_EDGE('',*,*,#551,.F.);
#699=ORIENTED_EDGE('',*,*,#558,.T.);
#700=ORIENTED_EDGE('',*,*,#559,.T.);
#701=ORIENTED_EDGE('',*,*,#560,.F.);
#702=ORIENTED_EDGE('',*,*,#561,.T.);
#703=ORIENTED_EDGE('',*,*,#562,.T.);
#704=ORIENTED_EDGE('',*,*,#563,.F.);
#705=ORIENTED_EDGE('',*,*,#564,.T.);
#706=ORIENTED_EDGE('',*,*,#565,.F.);
#707=ORIENTED_EDGE('',*,*,#566,.T.);
#708=ORIENTED_EDGE('',*,*,#567,.T.);
#709=ORIENTED_EDGE('',*,*,#568,.F.);
#710=ORIENTED_EDGE('',*,*,#569,.T.);
#711=ORIENTED_EDGE('',*,*,#570,.F.);
#712=ORIENTED_EDGE('',*,*,#571,.F.);
#713=ORIENTED_EDGE('',*,*,#552,.T.);
#714=ORIENTED_EDGE('',*,*,#560,.T.);
#715=ORIENTED_EDGE('',*,*,#572,.T.);
#716=ORIENTED_EDGE('',*,*,#573,.T.);
#717=ORIENTED_EDGE('',*,*,#574,.T.);
#718=ORIENTED_EDGE('',*,*,#563,.T.);
#719=ORIENTED_EDGE('',*,*,#575,.T.);
#720=ORIENTED_EDGE('',*,*,#576,.T.);
#721=ORIENTED_EDGE('',*,*,#577,.T.);
#722=ORIENTED_EDGE('',*,*,#578,.T.);
#723=ORIENTED_EDGE('',*,*,#554,.T.);
#724=ORIENTED_EDGE('',*,*,#546,.F.);
#725=ORIENTED_EDGE('',*,*,#550,.F.);
#726=ORIENTED_EDGE('',*,*,#579,.T.);
#727=ORIENTED_EDGE('',*,*,#556,.F.);
#728=ORIENTED_EDGE('',*,*,#580,.F.);
#729=ORIENTED_EDGE('',*,*,#581,.F.);
#730=ORIENTED_EDGE('',*,*,#570,.T.);
#731=ORIENTED_EDGE('',*,*,#582,.T.);
#732=ORIENTED_EDGE('',*,*,#565,.T.);
#733=ORIENTED_EDGE('',*,*,#583,.T.);
#734=ORIENTED_EDGE('',*,*,#561,.F.);
#735=ORIENTED_EDGE('',*,*,#584,.F.);
#736=ORIENTED_EDGE('',*,*,#585,.F.);
#737=ORIENTED_EDGE('',*,*,#586,.F.);
#738=ORIENTED_EDGE('',*,*,#558,.F.);
#739=ORIENTED_EDGE('',*,*,#544,.F.);
#740=ORIENTED_EDGE('',*,*,#577,.F.);
#741=ORIENTED_EDGE('',*,*,#587,.T.);
#742=ORIENTED_EDGE('',*,*,#568,.T.);
#743=ORIENTED_EDGE('',*,*,#581,.T.);
#744=ORIENTED_EDGE('',*,*,#588,.T.);
#745=ORIENTED_EDGE('',*,*,#574,.F.);
#746=ORIENTED_EDGE('',*,*,#589,.F.);
#747=ORIENTED_EDGE('',*,*,#584,.T.);
#748=ORIENTED_EDGE('',*,*,#564,.F.);
#749=ORIENTED_EDGE('',*,*,#573,.F.);
#750=ORIENTED_EDGE('',*,*,#590,.F.);
#751=ORIENTED_EDGE('',*,*,#585,.T.);
#752=ORIENTED_EDGE('',*,*,#589,.T.);
#753=ORIENTED_EDGE('',*,*,#572,.F.);
#754=ORIENTED_EDGE('',*,*,#559,.F.);
#755=ORIENTED_EDGE('',*,*,#586,.T.);
#756=ORIENTED_EDGE('',*,*,#590,.T.);
#757=ORIENTED_EDGE('',*,*,#555,.F.);
#758=ORIENTED_EDGE('',*,*,#578,.F.);
#759=ORIENTED_EDGE('',*,*,#588,.F.);
#760=ORIENTED_EDGE('',*,*,#580,.T.);
#761=ORIENTED_EDGE('',*,*,#567,.F.);
#762=ORIENTED_EDGE('',*,*,#591,.T.);
#763=ORIENTED_EDGE('',*,*,#575,.F.);
#764=ORIENTED_EDGE('',*,*,#562,.F.);
#765=ORIENTED_EDGE('',*,*,#583,.F.);
#766=ORIENTED_EDGE('',*,*,#566,.F.);
#767=ORIENTED_EDGE('',*,*,#582,.F.);
#768=ORIENTED_EDGE('',*,*,#569,.F.);
#769=ORIENTED_EDGE('',*,*,#587,.F.);
#770=ORIENTED_EDGE('',*,*,#576,.F.);
#771=ORIENTED_EDGE('',*,*,#591,.F.);
#772=ORIENTED_EDGE('',*,*,#553,.F.);
#773=ORIENTED_EDGE('',*,*,#571,.T.);
#774=ORIENTED_EDGE('',*,*,#547,.T.);
#775=ORIENTED_EDGE('',*,*,#579,.F.);
#776=ORIENTED_EDGE('',*,*,#549,.F.);
#777=ORIENTED_EDGE('',*,*,#557,.F.);
#778=ORIENTED_EDGE('',*,*,#592,.F.);
#779=ORIENTED_EDGE('',*,*,#593,.T.);
#780=ORIENTED_EDGE('',*,*,#594,.T.);
#781=ORIENTED_EDGE('',*,*,#593,.F.);
#782=ORIENTED_EDGE('',*,*,#592,.T.);
#783=ORIENTED_EDGE('',*,*,#594,.F.);
#784=ORIENTED_EDGE('',*,*,#595,.F.);
#785=ORIENTED_EDGE('',*,*,#596,.T.);
#786=ORIENTED_EDGE('',*,*,#597,.T.);
#787=ORIENTED_EDGE('',*,*,#598,.T.);
#788=ORIENTED_EDGE('',*,*,#599,.T.);
#789=ORIENTED_EDGE('',*,*,#600,.F.);
#790=ORIENTED_EDGE('',*,*,#601,.F.);
#791=ORIENTED_EDGE('',*,*,#596,.F.);
#792=ORIENTED_EDGE('',*,*,#595,.T.);
#793=ORIENTED_EDGE('',*,*,#602,.F.);
#794=ORIENTED_EDGE('',*,*,#603,.F.);
#795=ORIENTED_EDGE('',*,*,#599,.F.);
#796=ORIENTED_EDGE('',*,*,#601,.T.);
#797=ORIENTED_EDGE('',*,*,#604,.T.);
#798=ORIENTED_EDGE('',*,*,#605,.T.);
#799=ORIENTED_EDGE('',*,*,#597,.F.);
#800=ORIENTED_EDGE('',*,*,#605,.F.);
#801=ORIENTED_EDGE('',*,*,#606,.T.);
#802=ORIENTED_EDGE('',*,*,#602,.T.);
#803=ORIENTED_EDGE('',*,*,#598,.F.);
#804=ORIENTED_EDGE('',*,*,#603,.T.);
#805=ORIENTED_EDGE('',*,*,#606,.F.);
#806=ORIENTED_EDGE('',*,*,#604,.F.);
#807=ORIENTED_EDGE('',*,*,#600,.T.);
#808=ORIENTED_EDGE('',*,*,#607,.F.);
#809=ORIENTED_EDGE('',*,*,#608,.T.);
#810=ORIENTED_EDGE('',*,*,#609,.T.);
#811=ORIENTED_EDGE('',*,*,#608,.F.);
#812=ORIENTED_EDGE('',*,*,#610,.F.);
#813=ORIENTED_EDGE('',*,*,#611,.T.);
#814=ORIENTED_EDGE('',*,*,#612,.T.);
#815=ORIENTED_EDGE('',*,*,#611,.F.);
#816=ORIENTED_EDGE('',*,*,#612,.F.);
#817=ORIENTED_EDGE('',*,*,#607,.T.);
#818=ORIENTED_EDGE('',*,*,#610,.T.);
#819=ORIENTED_EDGE('',*,*,#609,.F.);
#820=ORIENTED_EDGE('',*,*,#613,.T.);
#821=ORIENTED_EDGE('',*,*,#614,.T.);
#822=ORIENTED_EDGE('',*,*,#615,.F.);
#823=ORIENTED_EDGE('',*,*,#614,.F.);
#824=ORIENTED_EDGE('',*,*,#616,.T.);
#825=ORIENTED_EDGE('',*,*,#617,.T.);
#826=ORIENTED_EDGE('',*,*,#618,.T.);
#827=ORIENTED_EDGE('',*,*,#619,.T.);
#828=ORIENTED_EDGE('',*,*,#620,.T.);
#829=ORIENTED_EDGE('',*,*,#621,.T.);
#830=ORIENTED_EDGE('',*,*,#613,.F.);
#831=ORIENTED_EDGE('',*,*,#622,.F.);
#832=ORIENTED_EDGE('',*,*,#623,.F.);
#833=ORIENTED_EDGE('',*,*,#624,.F.);
#834=ORIENTED_EDGE('',*,*,#625,.F.);
#835=ORIENTED_EDGE('',*,*,#626,.F.);
#836=ORIENTED_EDGE('',*,*,#627,.F.);
#837=ORIENTED_EDGE('',*,*,#615,.T.);
#838=ORIENTED_EDGE('',*,*,#622,.T.);
#839=ORIENTED_EDGE('',*,*,#628,.F.);
#840=ORIENTED_EDGE('',*,*,#616,.F.);
#841=ORIENTED_EDGE('',*,*,#629,.T.);
#842=ORIENTED_EDGE('',*,*,#627,.T.);
#843=ORIENTED_EDGE('',*,*,#630,.F.);
#844=ORIENTED_EDGE('',*,*,#617,.F.);
#845=ORIENTED_EDGE('',*,*,#628,.T.);
#846=ORIENTED_EDGE('',*,*,#626,.T.);
#847=ORIENTED_EDGE('',*,*,#631,.F.);
#848=ORIENTED_EDGE('',*,*,#618,.F.);
#849=ORIENTED_EDGE('',*,*,#630,.T.);
#850=ORIENTED_EDGE('',*,*,#625,.T.);
#851=ORIENTED_EDGE('',*,*,#632,.F.);
#852=ORIENTED_EDGE('',*,*,#619,.F.);
#853=ORIENTED_EDGE('',*,*,#631,.T.);
#854=ORIENTED_EDGE('',*,*,#624,.T.);
#855=ORIENTED_EDGE('',*,*,#633,.F.);
#856=ORIENTED_EDGE('',*,*,#620,.F.);
#857=ORIENTED_EDGE('',*,*,#632,.T.);
#858=ORIENTED_EDGE('',*,*,#623,.T.);
#859=ORIENTED_EDGE('',*,*,#629,.F.);
#860=ORIENTED_EDGE('',*,*,#621,.F.);
#861=ORIENTED_EDGE('',*,*,#633,.T.);
#862=CYLINDRICAL_SURFACE('',#1012,2.);
#863=CYLINDRICAL_SURFACE('',#1015,2.5);
#864=CYLINDRICAL_SURFACE('',#1025,2.);
#865=CYLINDRICAL_SURFACE('',#1041,2.65);
#866=CYLINDRICAL_SURFACE('',#1044,2.5);
#867=CYLINDRICAL_SURFACE('',#1068,6.);
#868=CYLINDRICAL_SURFACE('',#1079,6.);
#869=CYLINDRICAL_SURFACE('',#1082,7.);
#870=CYLINDRICAL_SURFACE('',#1089,2.);
#871=ADVANCED_FACE('',(#140),#862,.F.);
#872=ADVANCED_FACE('',(#141),#863,.T.);
#873=ADVANCED_FACE('',(#142,#92),#100,.T.);
#874=ADVANCED_FACE('',(#143,#93),#101,.F.);
#875=ADVANCED_FACE('',(#144),#63,.T.);
#876=ADVANCED_FACE('',(#145),#864,.T.);
#877=ADVANCED_FACE('',(#146),#102,.T.);
#878=ADVANCED_FACE('',(#147),#103,.F.);
#879=ADVANCED_FACE('',(#148),#59,.T.);
#880=ADVANCED_FACE('',(#149),#60,.T.);
#881=ADVANCED_FACE('',(#150),#61,.T.);
#882=ADVANCED_FACE('',(#151),#104,.F.);
#883=ADVANCED_FACE('',(#152),#62,.T.);
#884=ADVANCED_FACE('',(#153),#105,.F.);
#885=ADVANCED_FACE('',(#154),#865,.F.);
#886=ADVANCED_FACE('',(#155),#866,.T.);
#887=ADVANCED_FACE('',(#156),#106,.T.);
#888=ADVANCED_FACE('',(#157),#107,.F.);
#889=ADVANCED_FACE('',(#158),#108,.T.);
#890=ADVANCED_FACE('',(#159),#109,.T.);
#891=ADVANCED_FACE('',(#160,#94),#110,.F.);
#892=ADVANCED_FACE('',(#161,#95),#111,.T.);
#893=ADVANCED_FACE('',(#162),#112,.T.);
#894=ADVANCED_FACE('',(#163),#113,.T.);
#895=ADVANCED_FACE('',(#164),#114,.T.);
#896=ADVANCED_FACE('',(#165),#115,.T.);
#897=ADVANCED_FACE('',(#166),#116,.T.);
#898=ADVANCED_FACE('',(#167),#117,.T.);
#899=ADVANCED_FACE('',(#168),#118,.F.);
#900=ADVANCED_FACE('',(#169),#119,.F.);
#901=ADVANCED_FACE('',(#170),#120,.T.);
#902=ADVANCED_FACE('',(#171),#121,.F.);
#903=ADVANCED_FACE('',(#172),#867,.T.);
#904=ADVANCED_FACE('',(#173),#122,.T.);
#905=ADVANCED_FACE('',(#174,#96),#123,.F.);
#906=ADVANCED_FACE('',(#175),#124,.F.);
#907=ADVANCED_FACE('',(#176),#125,.T.);
#908=ADVANCED_FACE('',(#177),#126,.F.);
#909=ADVANCED_FACE('',(#178),#127,.F.);
#910=ADVANCED_FACE('',(#179),#128,.F.);
#911=ADVANCED_FACE('',(#180),#868,.F.);
#912=ADVANCED_FACE('',(#181),#869,.T.);
#913=ADVANCED_FACE('',(#182,#97),#129,.T.);
#914=ADVANCED_FACE('',(#183),#130,.T.);
#915=ADVANCED_FACE('',(#184),#131,.F.);
#916=ADVANCED_FACE('',(#185),#870,.F.);
#917=ADVANCED_FACE('',(#186,#98),#132,.T.);
#918=ADVANCED_FACE('',(#187,#99),#133,.F.);
#919=ADVANCED_FACE('',(#188),#134,.F.);
#920=ADVANCED_FACE('',(#189),#135,.F.);
#921=ADVANCED_FACE('',(#190),#136,.F.);
#922=ADVANCED_FACE('',(#191),#137,.F.);
#923=ADVANCED_FACE('',(#192),#138,.F.);
#924=ADVANCED_FACE('',(#193),#139,.F.);
#925=CLOSED_SHELL('',(#871,#872,#873,#874));
#926=CLOSED_SHELL('',(#875,#876,#877,#878));
#927=CLOSED_SHELL('',(#879,#880,#881,#882,#883,#884));
#928=CLOSED_SHELL('',(#885,#886,#887,#888,#889,#890,#891,#892,#893,#894,
#895,#896,#897,#898,#899,#900,#901,#902));
#929=CLOSED_SHELL('',(#903,#904,#905,#906,#907,#908,#909,#910));
#930=CLOSED_SHELL('',(#911,#912,#913,#914,#915));
#931=CLOSED_SHELL('',(#916,#917,#918,#919,#920,#921,#922,#923,#924));
#932=DERIVED_UNIT_ELEMENT(#946,1.);
#933=DERIVED_UNIT_ELEMENT(#5944,-3.);
#934=DERIVED_UNIT_ELEMENT(#946,1.);
#935=DERIVED_UNIT_ELEMENT(#5944,-3.);
#936=DERIVED_UNIT_ELEMENT(#946,1.);
#937=DERIVED_UNIT_ELEMENT(#5944,-3.);
#938=DERIVED_UNIT_ELEMENT(#946,1.);
#939=DERIVED_UNIT_ELEMENT(#5944,-3.);
#940=DERIVED_UNIT_ELEMENT(#946,1.);
#941=DERIVED_UNIT_ELEMENT(#5944,-3.);
#942=DERIVED_UNIT_ELEMENT(#946,1.);
#943=DERIVED_UNIT_ELEMENT(#5944,-3.);
#944=DERIVED_UNIT_ELEMENT(#946,1.);
#945=DERIVED_UNIT_ELEMENT(#5944,-3.);
#946=(
MASS_UNIT()
NAMED_UNIT(*)
SI_UNIT(.KILO.,.GRAM.)
);
#947=DERIVED_UNIT((#932,#933));
#948=DERIVED_UNIT((#934,#935));
#949=DERIVED_UNIT((#936,#937));
#950=DERIVED_UNIT((#938,#939));
#951=DERIVED_UNIT((#940,#941));
#952=DERIVED_UNIT((#942,#943));
#953=DERIVED_UNIT((#944,#945));
#954=MEASURE_REPRESENTATION_ITEM('density measure',
POSITIVE_RATIO_MEASURE(7850.),#947);
#955=MEASURE_REPRESENTATION_ITEM('density measure',
POSITIVE_RATIO_MEASURE(7850.),#948);
#956=MEASURE_REPRESENTATION_ITEM('density measure',
POSITIVE_RATIO_MEASURE(7850.),#949);
#957=MEASURE_REPRESENTATION_ITEM('density measure',
POSITIVE_RATIO_MEASURE(7850.),#950);
#958=MEASURE_REPRESENTATION_ITEM('density measure',
POSITIVE_RATIO_MEASURE(7850.),#951);
#959=MEASURE_REPRESENTATION_ITEM('density measure',
POSITIVE_RATIO_MEASURE(7850.),#952);
#960=MEASURE_REPRESENTATION_ITEM('density measure',
POSITIVE_RATIO_MEASURE(7850.),#953);
#961=PROPERTY_DEFINITION_REPRESENTATION(#996,#975);
#962=PROPERTY_DEFINITION_REPRESENTATION(#997,#976);
#963=PROPERTY_DEFINITION_REPRESENTATION(#998,#977);
#964=PROPERTY_DEFINITION_REPRESENTATION(#999,#978);
#965=PROPERTY_DEFINITION_REPRESENTATION(#1000,#979);
#966=PROPERTY_DEFINITION_REPRESENTATION(#1001,#980);
#967=PROPERTY_DEFINITION_REPRESENTATION(#1002,#981);
#968=PROPERTY_DEFINITION_REPRESENTATION(#1003,#982);
#969=PROPERTY_DEFINITION_REPRESENTATION(#1004,#983);
#970=PROPERTY_DEFINITION_REPRESENTATION(#1005,#984);
#971=PROPERTY_DEFINITION_REPRESENTATION(#1006,#985);
#972=PROPERTY_DEFINITION_REPRESENTATION(#1007,#986);
#973=PROPERTY_DEFINITION_REPRESENTATION(#1008,#987);
#974=PROPERTY_DEFINITION_REPRESENTATION(#1009,#988);
#975=REPRESENTATION('material name',(#989),#5935);
#976=REPRESENTATION('density',(#954),#5935);
#977=REPRESENTATION('material name',(#990),#5936);
#978=REPRESENTATION('density',(#955),#5936);
#979=REPRESENTATION('material name',(#991),#5937);
#980=REPRESENTATION('density',(#956),#5937);
#981=REPRESENTATION('material name',(#992),#5938);
#982=REPRESENTATION('density',(#957),#5938);
#983=REPRESENTATION('material name',(#993),#5939);
#984=REPRESENTATION('density',(#958),#5939);
#985=REPRESENTATION('material name',(#994),#5940);
#986=REPRESENTATION('density',(#959),#5940);
#987=REPRESENTATION('material name',(#995),#5941);
#988=REPRESENTATION('density',(#960),#5941);
#989=DESCRIPTIVE_REPRESENTATION_ITEM('Steel','Steel');
#990=DESCRIPTIVE_REPRESENTATION_ITEM('Steel','Steel');
#991=DESCRIPTIVE_REPRESENTATION_ITEM('Steel','Steel');
#992=DESCRIPTIVE_REPRESENTATION_ITEM('Steel','Steel');
#993=DESCRIPTIVE_REPRESENTATION_ITEM('Steel','Steel');
#994=DESCRIPTIVE_REPRESENTATION_ITEM('Steel','Steel');
#995=DESCRIPTIVE_REPRESENTATION_ITEM('Steel','Steel');
#996=PROPERTY_DEFINITION('material property','material name',#5984);
#997=PROPERTY_DEFINITION('material property','density of part',#5984);
#998=PROPERTY_DEFINITION('material property','material name',#5985);
#999=PROPERTY_DEFINITION('material property','density of part',#5985);
#1000=PROPERTY_DEFINITION('material property','material name',#5986);
#1001=PROPERTY_DEFINITION('material property','density of part',#5986);
#1002=PROPERTY_DEFINITION('material property','material name',#5987);
#1003=PROPERTY_DEFINITION('material property','density of part',#5987);
#1004=PROPERTY_DEFINITION('material property','material name',#5988);
#1005=PROPERTY_DEFINITION('material property','density of part',#5988);
#1006=PROPERTY_DEFINITION('material property','material name',#5989);
#1007=PROPERTY_DEFINITION('material property','density of part',#5989);
#1008=PROPERTY_DEFINITION('material property','material name',#5990);
#1009=PROPERTY_DEFINITION('material property','density of part',#5990);
#1010=AXIS2_PLACEMENT_3D('',#1391,#1111,#1112);
#1011=AXIS2_PLACEMENT_3D('',#1392,#1113,#1114);
#1012=AXIS2_PLACEMENT_3D('',#1393,#1115,#1116);
#1013=AXIS2_PLACEMENT_3D('',#1395,#1117,#1118);
#1014=AXIS2_PLACEMENT_3D('',#1398,#1120,#1121);
#1015=AXIS2_PLACEMENT_3D('',#1399,#1122,#1123);
#1016=AXIS2_PLACEMENT_3D('',#1401,#1124,#1125);
#1017=AXIS2_PLACEMENT_3D('',#1404,#1127,#1128);
#1018=AXIS2_PLACEMENT_3D('',#1405,#1129,#1130);
#1019=AXIS2_PLACEMENT_3D('',#1406,#1131,#1132);
#1020=AXIS2_PLACEMENT_3D('',#1407,#1133,#1134);
#1021=AXIS2_PLACEMENT_3D('',#1408,#1135,#1136);
#1022=AXIS2_PLACEMENT_3D('',#1411,#1137,#1138);
#1023=AXIS2_PLACEMENT_3D('',#1412,#1139,#1140);
#1024=AXIS2_PLACEMENT_3D('',#1415,#1142,#1143);
#1025=AXIS2_PLACEMENT_3D('',#1416,#1144,#1145);
#1026=AXIS2_PLACEMENT_3D('',#1419,#1147,#1148);
#1027=AXIS2_PLACEMENT_3D('',#1420,#1149,#1150);
#1028=AXIS2_PLACEMENT_3D('',#1421,#1151,#1152);
#1029=AXIS2_PLACEMENT_3D('',#1422,#1153,#1154);
#1030=AXIS2_PLACEMENT_3D('',#2153,#1155,#1156);
#1031=AXIS2_PLACEMENT_3D('',#2310,#1157,#1158);
#1032=AXIS2_PLACEMENT_3D('',#2312,#1159,#1160);
#1033=AXIS2_PLACEMENT_3D('',#3376,#1161,#1162);
#1034=AXIS2_PLACEMENT_3D('',#3571,#1163,#1164);
#1035=AXIS2_PLACEMENT_3D('',#4675,#1165,#1166);
#1036=AXIS2_PLACEMENT_3D('',#4676,#1167,#1168);
#1037=AXIS2_PLACEMENT_3D('',#4677,#1169,#1170);
#1038=AXIS2_PLACEMENT_3D('',#5718,#1171,#1172);
#1039=AXIS2_PLACEMENT_3D('',#5719,#1173,#1174);
#1040=AXIS2_PLACEMENT_3D('',#5720,#1175,#1176);
#1041=AXIS2_PLACEMENT_3D('',#5721,#1177,#1178);
#1042=AXIS2_PLACEMENT_3D('',#5723,#1179,#1180);
#1043=AXIS2_PLACEMENT_3D('',#5726,#1182,#1183);
#1044=AXIS2_PLACEMENT_3D('',#5727,#1184,#1185);
#1045=AXIS2_PLACEMENT_3D('',#5729,#1186,#1187);
#1046=AXIS2_PLACEMENT_3D('',#5733,#1189,#1190);
#1047=AXIS2_PLACEMENT_3D('',#5737,#1192,#1193);
#1048=AXIS2_PLACEMENT_3D('',#5741,#1195,#1196);
#1049=AXIS2_PLACEMENT_3D('',#5745,#1198,#1199);
#1050=AXIS2_PLACEMENT_3D('',#5748,#1201,#1202);
#1051=AXIS2_PLACEMENT_3D('',#5749,#1203,#1204);
#1052=AXIS2_PLACEMENT_3D('',#5755,#1208,#1209);
#1053=AXIS2_PLACEMENT_3D('',#5764,#1214,#1215);
#1054=AXIS2_PLACEMENT_3D('',#5771,#1219,#1220);
#1055=AXIS2_PLACEMENT_3D('',#5778,#1224,#1225);
#1056=AXIS2_PLACEMENT_3D('',#5792,#1234,#1235);
#1057=AXIS2_PLACEMENT_3D('',#5804,#1244,#1245);
#1058=AXIS2_PLACEMENT_3D('',#5807,#1248,#1249);
#1059=AXIS2_PLACEMENT_3D('',#5809,#1251,#1252);
#1060=AXIS2_PLACEMENT_3D('',#5811,#1254,#1255);
#1061=AXIS2_PLACEMENT_3D('',#5812,#1256,#1257);
#1062=AXIS2_PLACEMENT_3D('',#5813,#1258,#1259);
#1063=AXIS2_PLACEMENT_3D('',#5815,#1261,#1262);
#1064=AXIS2_PLACEMENT_3D('',#5816,#1263,#1264);
#1065=AXIS2_PLACEMENT_3D('',#5817,#1265,#1266);
#1066=AXIS2_PLACEMENT_3D('',#5818,#1267,#1268);
#1067=AXIS2_PLACEMENT_3D('',#5819,#1269,#1270);
#1068=AXIS2_PLACEMENT_3D('',#5820,#1271,#1272);
#1069=AXIS2_PLACEMENT_3D('',#5822,#1273,#1274);
#1070=AXIS2_PLACEMENT_3D('',#5825,#1276,#1277);
#1071=AXIS2_PLACEMENT_3D('',#5826,#1278,#1279);
#1072=AXIS2_PLACEMENT_3D('',#5827,#1280,#1281);
#1073=AXIS2_PLACEMENT_3D('',#5836,#1286,#1287);
#1074=AXIS2_PLACEMENT_3D('',#5842,#1291,#1292);
#1075=AXIS2_PLACEMENT_3D('',#5846,#1295,#1296);
#1076=AXIS2_PLACEMENT_3D('',#5850,#1299,#1300);
#1077=AXIS2_PLACEMENT_3D('',#5852,#1302,#1303);
#1078=AXIS2_PLACEMENT_3D('',#5853,#1304,#1305);
#1079=AXIS2_PLACEMENT_3D('',#5854,#1306,#1307);
#1080=AXIS2_PLACEMENT_3D('',#5856,#1308,#1309);
#1081=AXIS2_PLACEMENT_3D('',#5859,#1311,#1312);
#1082=AXIS2_PLACEMENT_3D('',#5860,#1313,#1314);
#1083=AXIS2_PLACEMENT_3D('',#5862,#1315,#1316);
#1084=AXIS2_PLACEMENT_3D('',#5865,#1318,#1319);
#1085=AXIS2_PLACEMENT_3D('',#5866,#1320,#1321);
#1086=AXIS2_PLACEMENT_3D('',#5867,#1322,#1323);
#1087=AXIS2_PLACEMENT_3D('',#5868,#1324,#1325);
#1088=AXIS2_PLACEMENT_3D('',#5869,#1326,#1327);
#1089=AXIS2_PLACEMENT_3D('',#5870,#1328,#1329);
#1090=AXIS2_PLACEMENT_3D('',#5872,#1330,#1331);
#1091=AXIS2_PLACEMENT_3D('',#5875,#1333,#1334);
#1092=AXIS2_PLACEMENT_3D('',#5876,#1335,#1336);
#1093=AXIS2_PLACEMENT_3D('',#5889,#1343,#1344);
#1094=AXIS2_PLACEMENT_3D('',#5902,#1351,#1352);
#1095=AXIS2_PLACEMENT_3D('',#5905,#1355,#1356);
#1096=AXIS2_PLACEMENT_3D('',#5907,#1358,#1359);
#1097=AXIS2_PLACEMENT_3D('',#5909,#1361,#1362);
#1098=AXIS2_PLACEMENT_3D('',#5911,#1364,#1365);
#1099=AXIS2_PLACEMENT_3D('',#5913,#1367,#1368);
#1100=AXIS2_PLACEMENT_3D('',#5914,#1369,#1370);
#1101=AXIS2_PLACEMENT_3D('',#5915,#1371,#1372);
#1102=AXIS2_PLACEMENT_3D('',#5916,#1373,#1374);
#1103=AXIS2_PLACEMENT_3D('',#5917,#1375,#1376);
#1104=AXIS2_PLACEMENT_3D('',#5918,#1377,#1378);
#1105=AXIS2_PLACEMENT_3D('',#5919,#1379,#1380);
#1106=AXIS2_PLACEMENT_3D('',#5920,#1381,#1382);
#1107=AXIS2_PLACEMENT_3D('',#5921,#1383,#1384);
#1108=AXIS2_PLACEMENT_3D('',#5922,#1385,#1386);
#1109=AXIS2_PLACEMENT_3D('',#5923,#1387,#1388);
#1110=AXIS2_PLACEMENT_3D('',#5924,#1389,#1390);
#1111=DIRECTION('axis',(0.,0.,1.));
#1112=DIRECTION('refdir',(1.,0.,0.));
#1113=DIRECTION('axis',(0.,0.,1.));
#1114=DIRECTION('refdir',(1.,0.,0.));
#1115=DIRECTION('center_axis',(0.,0.,-1.));
#1116=DIRECTION('ref_axis',(-1.,0.,0.));
#1117=DIRECTION('center_axis',(0.,0.,1.));
#1118=DIRECTION('ref_axis',(1.,0.,0.));
#1119=DIRECTION('',(0.,0.,-1.));
#1120=DIRECTION('center_axis',(0.,0.,1.));
#1121=DIRECTION('ref_axis',(1.,0.,0.));
#1122=DIRECTION('center_axis',(0.,0.,-1.));
#1123=DIRECTION('ref_axis',(-1.,0.,0.));
#1124=DIRECTION('center_axis',(0.,0.,1.));
#1125=DIRECTION('ref_axis',(1.,0.,0.));
#1126=DIRECTION('',(0.,0.,1.));
#1127=DIRECTION('center_axis',(0.,0.,1.));
#1128=DIRECTION('ref_axis',(1.,0.,0.));
#1129=DIRECTION('center_axis',(0.,0.,1.));
#1130=DIRECTION('ref_axis',(1.,0.,0.));
#1131=DIRECTION('center_axis',(0.,0.,1.));
#1132=DIRECTION('ref_axis',(1.,0.,0.));
#1133=DIRECTION('axis',(0.,0.,1.));
#1134=DIRECTION('refdir',(1.,0.,0.));
#1135=DIRECTION('center_axis',(0.,0.,1.));
#1136=DIRECTION('ref_axis',(1.,0.,0.));
#1137=DIRECTION('center_axis',(0.,0.,1.));
#1138=DIRECTION('ref_axis',(1.,0.,0.));
#1139=DIRECTION('center_axis',(0.,0.,1.));
#1140=DIRECTION('ref_axis',(1.,0.,0.));
#1141=DIRECTION('',(0.70710678118656,8.65956056235509E-17,-0.707106781186535));
#1142=DIRECTION('center_axis',(0.,0.,1.));
#1143=DIRECTION('ref_axis',(1.,0.,0.));
#1144=DIRECTION('center_axis',(0.,0.,-1.));
#1145=DIRECTION('ref_axis',(-1.,0.,0.));
#1146=DIRECTION('',(0.,0.,1.));
#1147=DIRECTION('center_axis',(0.,0.,1.));
#1148=DIRECTION('ref_axis',(1.,0.,0.));
#1149=DIRECTION('center_axis',(0.,0.,1.));
#1150=DIRECTION('ref_axis',(1.,0.,0.));
#1151=DIRECTION('center_axis',(0.,0.,1.));
#1152=DIRECTION('ref_axis',(1.,0.,0.));
#1153=DIRECTION('axis',(0.,0.,1.));
#1154=DIRECTION('refdir',(1.,0.,0.));
#1155=DIRECTION('center_axis',(-0.0122214764460586,-0.994958909981894,-0.0995359380380735));
#1156=DIRECTION('ref_axis',(2.2423307198858E-17,0.0995433724380481,-0.995033224070262));
#1157=DIRECTION('center_axis',(-0.0122214764459953,0.994958909981895,0.0995359380380777));
#1158=DIRECTION('ref_axis',(-6.9485554107327E-15,-0.0995433724380523,0.995033224070262));
#1159=DIRECTION('center_axis',(-0.0122214764459953,0.994958909981895,0.0995359380380777));
#1160=DIRECTION('ref_axis',(-6.9485554107327E-15,-0.0995433724380523,0.995033224070262));
#1161=DIRECTION('center_axis',(-0.0122214764460684,0.994958909981894,0.0995359380380777));
#1162=DIRECTION('ref_axis',(-1.06054523794617E-17,-0.0995433724380524,0.995033224070262));
#1163=DIRECTION('center_axis',(-0.0122214764459953,0.994958909981895,0.0995359380380777));
#1164=DIRECTION('ref_axis',(-6.9485554107327E-15,-0.0995433724380523,0.995033224070262));
#1165=DIRECTION('center_axis',(-0.0122214764460684,0.994958909981894,0.0995359380380777));
#1166=DIRECTION('ref_axis',(-1.06054523794617E-17,-0.0995433724380524,0.995033224070262));
#1167=DIRECTION('center_axis',(-0.0122214764459953,0.994958909981895,0.0995359380380777));
#1168=DIRECTION('ref_axis',(-6.9485554107327E-15,-0.0995433724380523,0.995033224070262));
#1169=DIRECTION('center_axis',(-0.0122214764460684,0.994958909981894,0.0995359380380777));
#1170=DIRECTION('ref_axis',(-6.86173012619271E-20,-0.0995433724380523,0.995033224070262));
#1171=DIRECTION('center_axis',(-0.0122214764460586,-0.994958909981894,-0.0995359380380735));
#1172=DIRECTION('ref_axis',(2.2423307198858E-17,0.0995433724380481,-0.995033224070262));
#1173=DIRECTION('center_axis',(-0.0122214764460586,-0.994958909981894,-0.0995359380380735));
#1174=DIRECTION('ref_axis',(-8.78275546101855E-20,0.0995433724380481,-0.995033224070262));
#1175=DIRECTION('axis',(0.,0.,1.));
#1176=DIRECTION('refdir',(1.,0.,0.));
#1177=DIRECTION('center_axis',(0.,0.,1.));
#1178=DIRECTION('ref_axis',(1.,0.,0.));
#1179=DIRECTION('center_axis',(0.,0.,-1.));
#1180=DIRECTION('ref_axis',(-1.,0.,0.));
#1181=DIRECTION('',(0.,0.,1.));
#1182=DIRECTION('center_axis',(0.,0.,1.));
#1183=DIRECTION('ref_axis',(1.,0.,0.));
#1184=DIRECTION('center_axis',(-1.,0.,0.));
#1185=DIRECTION('ref_axis',(0.,0.,1.));
#1186=DIRECTION('center_axis',(-1.,0.,0.));
#1187=DIRECTION('ref_axis',(0.,0.,1.));
#1188=DIRECTION('',(1.,0.,0.));
#1189=DIRECTION('center_axis',(-1.,0.,0.));
#1190=DIRECTION('ref_axis',(0.,0.,1.));
#1191=DIRECTION('',(-1.,0.,0.));
#1192=DIRECTION('center_axis',(-1.,-1.51313062618285E-16,0.));
#1193=DIRECTION('ref_axis',(1.51313062618285E-16,-1.,0.));
#1194=DIRECTION('',(-1.,0.,0.));
#1195=DIRECTION('center_axis',(-1.,0.,0.));
#1196=DIRECTION('ref_axis',(0.,0.,1.));
#1197=DIRECTION('',(1.,0.,0.));
#1198=DIRECTION('center_axis',(-1.,-1.51313062618285E-16,0.));
#1199=DIRECTION('ref_axis',(1.51313062618285E-16,-1.,0.));
#1200=DIRECTION('',(1.,0.,0.));
#1201=DIRECTION('center_axis',(-1.,0.,0.));
#1202=DIRECTION('ref_axis',(0.,0.,1.));
#1203=DIRECTION('center_axis',(-1.,-1.51313062618285E-16,0.));
#1204=DIRECTION('ref_axis',(1.51313062618285E-16,-1.,0.));
#1205=DIRECTION('',(1.51313062618285E-16,-1.,0.));
#1206=DIRECTION('',(0.,0.,1.));
#1207=DIRECTION('',(1.51313062618285E-16,-1.,0.));
#1208=DIRECTION('center_axis',(-1.,0.,0.));
#1209=DIRECTION('ref_axis',(0.,0.,1.));
#1210=DIRECTION('',(0.,1.,0.));
#1211=DIRECTION('',(0.,0.,1.));
#1212=DIRECTION('',(0.,1.,0.));
#1213=DIRECTION('',(0.,0.,-1.));
#1214=DIRECTION('center_axis',(0.,1.,0.));
#1215=DIRECTION('ref_axis',(0.,0.,1.));
#1216=DIRECTION('',(1.,0.,0.));
#1217=DIRECTION('',(0.866413978654257,0.,0.499326363806779));
#1218=DIRECTION('',(0.,0.,-1.));
#1219=DIRECTION('center_axis',(-1.,0.,0.));
#1220=DIRECTION('ref_axis',(0.,0.,1.));
#1221=DIRECTION('',(0.,0.,-1.));
#1222=DIRECTION('',(0.,0.999402687851137,-0.0345581758188068));
#1223=DIRECTION('',(0.,1.,0.));
#1224=DIRECTION('center_axis',(0.,0.,-1.));
#1225=DIRECTION('ref_axis',(-1.,0.,0.));
#1226=DIRECTION('',(0.,1.,0.));
#1227=DIRECTION('',(1.,0.,0.));
#1228=DIRECTION('',(-6.93889390390723E-17,1.,0.));
#1229=DIRECTION('',(-0.707106781186544,0.707106781186551,0.));
#1230=DIRECTION('',(-0.17364817766693,0.984807753012208,0.));
#1231=DIRECTION('',(-0.0598922907279467,-0.998204845465779,0.));
#1232=DIRECTION('',(0.611809881784581,-0.791004847362351,0.));
#1233=DIRECTION('',(1.51313062618285E-16,-1.,0.));
#1234=DIRECTION('center_axis',(0.,0.,-1.));
#1235=DIRECTION('ref_axis',(-1.,0.,0.));
#1236=DIRECTION('',(0.,1.,0.));
#1237=DIRECTION('',(1.51313062618285E-16,-1.,0.));
#1238=DIRECTION('',(0.611809881784581,-0.791004847362351,0.));
#1239=DIRECTION('',(0.0598922907279467,0.998204845465779,0.));
#1240=DIRECTION('',(0.17364817766693,-0.984807753012208,0.));
#1241=DIRECTION('',(-0.707106781186544,0.707106781186551,0.));
#1242=DIRECTION('',(-6.93889390390723E-17,1.,0.));
#1243=DIRECTION('',(1.,0.,0.));
#1244=DIRECTION('center_axis',(-0.791004847362351,-0.611809881784581,0.));
#1245=DIRECTION('ref_axis',(0.611809881784581,-0.791004847362351,0.));
#1246=DIRECTION('',(-0.571919987099744,0.739431473025142,-0.355174077116697));
#1247=DIRECTION('',(0.,0.,1.));
#1248=DIRECTION('center_axis',(0.707106781186551,0.707106781186544,0.));
#1249=DIRECTION('ref_axis',(-0.707106781186544,0.707106781186551,0.));
#1250=DIRECTION('',(0.,0.,1.));
#1251=DIRECTION('center_axis',(1.,6.93889390390723E-17,0.));
#1252=DIRECTION('ref_axis',(-6.93889390390723E-17,1.,0.));
#1253=DIRECTION('',(0.,0.,1.));
#1254=DIRECTION('center_axis',(0.,-1.,0.));
#1255=DIRECTION('ref_axis',(0.,0.,-1.));
#1256=DIRECTION('center_axis',(-1.,-1.51313062618285E-16,0.));
#1257=DIRECTION('ref_axis',(1.51313062618285E-16,-1.,0.));
#1258=DIRECTION('center_axis',(0.984807753012208,0.17364817766693,0.));
#1259=DIRECTION('ref_axis',(0.,0.,1.));
#1260=DIRECTION('',(0.172106918435043,-0.976066837551089,0.132938847820377));
#1261=DIRECTION('center_axis',(0.499102422732889,-0.0299461453639734,-0.866025403784439));
#1262=DIRECTION('ref_axis',(-0.0598922907279467,-0.998204845465779,1.0301470331017E-18));
#1263=DIRECTION('center_axis',(-1.,0.,0.));
#1264=DIRECTION('ref_axis',(0.,0.,1.));
#1265=DIRECTION('center_axis',(-1.,0.,0.));
#1266=DIRECTION('ref_axis',(0.,0.,1.));
#1267=DIRECTION('center_axis',(-1.,0.,0.));
#1268=DIRECTION('ref_axis',(0.,0.,1.));
#1269=DIRECTION('axis',(0.,0.,1.));
#1270=DIRECTION('refdir',(1.,0.,0.));
#1271=DIRECTION('center_axis',(1.04083408558608E-16,-1.,0.));
#1272=DIRECTION('ref_axis',(1.,1.04083408558608E-16,0.));
#1273=DIRECTION('center_axis',(1.04083408558608E-16,-1.,0.));
#1274=DIRECTION('ref_axis',(1.,1.04083408558608E-16,0.));
#1275=DIRECTION('',(-1.04083408558608E-16,1.,0.));
#1276=DIRECTION('center_axis',(1.04083408558608E-16,-1.,0.));
#1277=DIRECTION('ref_axis',(1.,1.04083408558608E-16,0.));
#1278=DIRECTION('center_axis',(1.04083408558608E-16,-1.,0.));
#1279=DIRECTION('ref_axis',(1.,1.04083408558608E-16,0.));
#1280=DIRECTION('center_axis',(1.04083408558608E-16,-1.,0.));
#1281=DIRECTION('ref_axis',(1.,1.04083408558608E-16,0.));
#1282=DIRECTION('',(1.,1.04083408558608E-16,0.));
#1283=DIRECTION('',(0.,0.,-1.));
#1284=DIRECTION('',(1.,1.04083408558608E-16,0.));
#1285=DIRECTION('',(0.,0.,1.));
#1286=DIRECTION('center_axis',(-1.,-1.51313062618285E-16,0.));
#1287=DIRECTION('ref_axis',(1.51313062618285E-16,-1.,0.));
#1288=DIRECTION('',(1.51313062618285E-16,-1.,0.));
#1289=DIRECTION('',(0.,0.,1.));
#1290=DIRECTION('',(1.51313062618285E-16,-1.,0.));
#1291=DIRECTION('center_axis',(0.,0.,-1.));
#1292=DIRECTION('ref_axis',(-1.,0.,0.));
#1293=DIRECTION('',(-6.93889390390723E-17,1.,0.));
#1294=DIRECTION('',(1.,0.,0.));
#1295=DIRECTION('center_axis',(0.,0.,-1.));
#1296=DIRECTION('ref_axis',(-1.,0.,0.));
#1297=DIRECTION('',(1.,0.,0.));
#1298=DIRECTION('',(-6.93889390390723E-17,1.,0.));
#1299=DIRECTION('center_axis',(1.,6.93889390390723E-17,0.));
#1300=DIRECTION('ref_axis',(-6.93889390390723E-17,1.,0.));
#1301=DIRECTION('',(0.,0.,1.));
#1302=DIRECTION('center_axis',(0.,-1.,0.));
#1303=DIRECTION('ref_axis',(0.,0.,-1.));
#1304=DIRECTION('axis',(0.,0.,1.));
#1305=DIRECTION('refdir',(1.,0.,0.));
#1306=DIRECTION('center_axis',(1.38777878078145E-16,-1.,0.));
#1307=DIRECTION('ref_axis',(1.,1.38777878078145E-16,0.));
#1308=DIRECTION('center_axis',(1.56125112837913E-16,-1.,0.));
#1309=DIRECTION('ref_axis',(1.,1.56125112837913E-16,0.));
#1310=DIRECTION('',(1.38777878078145E-16,-1.,0.));
#1311=DIRECTION('center_axis',(1.56125112837913E-16,-1.,0.));
#1312=DIRECTION('ref_axis',(1.,1.56125112837913E-16,0.));
#1313=DIRECTION('center_axis',(1.38777878078145E-16,-1.,0.));
#1314=DIRECTION('ref_axis',(1.,1.38777878078145E-16,0.));
#1315=DIRECTION('center_axis',(1.56125112837913E-16,-1.,0.));
#1316=DIRECTION('ref_axis',(1.,1.56125112837913E-16,0.));
#1317=DIRECTION('',(-1.38777878078145E-16,1.,0.));
#1318=DIRECTION('center_axis',(1.38777878078145E-16,-1.,0.));
#1319=DIRECTION('ref_axis',(1.,1.38777878078145E-16,0.));
#1320=DIRECTION('center_axis',(-1.56125112837913E-16,1.,0.));
#1321=DIRECTION('ref_axis',(-1.,-1.56125112837913E-16,0.));
#1322=DIRECTION('center_axis',(1.56125112837913E-16,-1.,0.));
#1323=DIRECTION('ref_axis',(1.,1.56125112837913E-16,0.));
#1324=DIRECTION('center_axis',(1.56125112837913E-16,-1.,0.));
#1325=DIRECTION('ref_axis',(1.,1.56125112837913E-16,0.));
#1326=DIRECTION('axis',(0.,0.,1.));
#1327=DIRECTION('refdir',(1.,0.,0.));
#1328=DIRECTION('center_axis',(0.,0.,-1.));
#1329=DIRECTION('ref_axis',(-1.,0.,0.));
#1330=DIRECTION('center_axis',(0.,0.,1.));
#1331=DIRECTION('ref_axis',(1.,0.,0.));
#1332=DIRECTION('',(0.,0.,-1.));
#1333=DIRECTION('center_axis',(0.,0.,1.));
#1334=DIRECTION('ref_axis',(1.,0.,0.));
#1335=DIRECTION('center_axis',(0.,0.,1.));
#1336=DIRECTION('ref_axis',(1.,0.,0.));
#1337=DIRECTION('',(0.,1.,0.));
#1338=DIRECTION('',(-0.866025403784439,0.5,0.));
#1339=DIRECTION('',(-0.866025403784438,-0.5,0.));
#1340=DIRECTION('',(0.,-1.,0.));
#1341=DIRECTION('',(0.866025403784438,-0.5,0.));
#1342=DIRECTION('',(0.866025403784438,0.5,0.));
#1343=DIRECTION('center_axis',(0.,0.,1.));
#1344=DIRECTION('ref_axis',(1.,0.,0.));
#1345=DIRECTION('',(0.,1.,0.));
#1346=DIRECTION('',(0.866025403784438,0.5,0.));
#1347=DIRECTION('',(0.866025403784438,-0.5,0.));
#1348=DIRECTION('',(0.,-1.,0.));
#1349=DIRECTION('',(-0.866025403784438,-0.5,0.));
#1350=DIRECTION('',(-0.866025403784439,0.5,0.));
#1351=DIRECTION('center_axis',(-1.,0.,0.));
#1352=DIRECTION('ref_axis',(0.,0.,1.));
#1353=DIRECTION('',(0.,0.,-1.));
#1354=DIRECTION('',(0.,0.,-1.));
#1355=DIRECTION('center_axis',(-0.5,-0.866025403784439,0.));
#1356=DIRECTION('ref_axis',(0.866025403784439,-0.5,0.));
#1357=DIRECTION('',(0.,0.,-1.));
#1358=DIRECTION('center_axis',(0.5,-0.866025403784439,0.));
#1359=DIRECTION('ref_axis',(0.866025403784439,0.5,0.));
#1360=DIRECTION('',(0.,0.,-1.));
#1361=DIRECTION('center_axis',(1.,0.,0.));
#1362=DIRECTION('ref_axis',(0.,0.,-1.));
#1363=DIRECTION('',(0.,0.,-1.));
#1364=DIRECTION('center_axis',(0.5,0.866025403784439,0.));
#1365=DIRECTION('ref_axis',(-0.866025403784439,0.5,0.));
#1366=DIRECTION('',(0.,0.,-1.));
#1367=DIRECTION('center_axis',(-0.5,0.866025403784438,0.));
#1368=DIRECTION('ref_axis',(-0.866025403784438,-0.5,0.));
#1369=DIRECTION('',(0.,0.,1.));
#1370=DIRECTION('',(1.,0.,0.));
#1371=DIRECTION('',(0.,0.,1.));
#1372=DIRECTION('',(1.,0.,0.));
#1373=DIRECTION('',(0.,0.,1.));
#1374=DIRECTION('',(1.,0.,0.));
#1375=DIRECTION('',(0.,0.,1.));
#1376=DIRECTION('',(1.,0.,0.));
#1377=DIRECTION('',(0.,0.,1.));
#1378=DIRECTION('',(1.,0.,0.));
#1379=DIRECTION('',(0.,0.,1.));
#1380=DIRECTION('',(1.,0.,0.));
#1381=DIRECTION('',(1.,0.,0.));
#1382=DIRECTION('',(0.,0.,-1.));
#1383=DIRECTION('',(3.43071521274429E-17,-5.57899232955203E-17,-1.));
#1384=DIRECTION('',(-1.,-5.55111512312578E-17,-3.43071521274429E-17));
#1385=DIRECTION('',(0.,0.,-1.));
#1386=DIRECTION('',(-1.,0.,0.));
#1387=DIRECTION('',(0.,0.,-1.));
#1388=DIRECTION('',(-1.,0.,0.));
#1389=DIRECTION('',(0.,0.,1.));
#1390=DIRECTION('',(1.,0.,0.));
#1391=CARTESIAN_POINT('',(0.,0.,0.));
#1392=CARTESIAN_POINT('',(0.,0.,0.));
#1393=CARTESIAN_POINT('Origin',(0.,0.,2.));
#1394=CARTESIAN_POINT('',(2.,-2.44929359829471E-16,2.));
#1395=CARTESIAN_POINT('Origin',(0.,0.,2.));
#1396=CARTESIAN_POINT('',(2.,-2.44929359829471E-16,-2.));
#1397=CARTESIAN_POINT('',(2.,-2.44929359829471E-16,2.));
#1398=CARTESIAN_POINT('Origin',(0.,0.,-2.));
#1399=CARTESIAN_POINT('Origin',(0.,0.,2.));
#1400=CARTESIAN_POINT('',(2.5,-3.06161699786838E-16,-2.));
#1401=CARTESIAN_POINT('Origin',(0.,0.,-2.));
#1402=CARTESIAN_POINT('',(2.5,-3.06161699786838E-16,2.));
#1403=CARTESIAN_POINT('',(2.5,-3.06161699786838E-16,2.));
#1404=CARTESIAN_POINT('Origin',(0.,0.,2.));
#1405=CARTESIAN_POINT('Origin',(0.,0.,2.));
#1406=CARTESIAN_POINT('Origin',(0.,0.,-2.));
#1407=CARTESIAN_POINT('',(0.,0.,0.));
#1408=CARTESIAN_POINT('Origin',(0.,0.,-6.));
#1409=CARTESIAN_POINT('',(2.,2.44929359829471E-16,-5.61000000000001));
#1410=CARTESIAN_POINT('',(-2.,-2.44929359829471E-16,-5.61000000000001));
#1411=CARTESIAN_POINT('Origin',(0.,0.,-5.61000000000001));
#1412=CARTESIAN_POINT('Origin',(0.,0.,-5.61000000000001));
#1413=CARTESIAN_POINT('',(-1.61,-1.97168134662724E-16,-6.));
#1414=CARTESIAN_POINT('',(-1.61,-1.97168134662724E-16,-6.));
#1415=CARTESIAN_POINT('Origin',(0.,0.,-6.));
#1416=CARTESIAN_POINT('Origin',(0.,0.,6.));
#1417=CARTESIAN_POINT('',(2.,-2.44929359829471E-16,6.));
#1418=CARTESIAN_POINT('',(2.,-2.44929359829471E-16,6.));
#1419=CARTESIAN_POINT('Origin',(0.,0.,6.));
#1420=CARTESIAN_POINT('Origin',(0.,0.,6.));
#1421=CARTESIAN_POINT('Origin',(0.,0.,-6.));
#1422=CARTESIAN_POINT('',(0.,0.,0.));
#1423=CARTESIAN_POINT('Ctrl Pts',(-3.5,-27.1131792176833,21.5024833879649));
#1424=CARTESIAN_POINT('Ctrl Pts',(-3.51479119919922,-27.6859453885664,21.4451837185487));
#1425=CARTESIAN_POINT('Ctrl Pts',(-3.3869826954375,-28.2639018202575,21.3878808596267));
#1426=CARTESIAN_POINT('Ctrl Pts',(-2.61104013965461,-29.8091522948055,21.2159741435134));
#1427=CARTESIAN_POINT('Ctrl Pts',(-1.55527081107218,-30.5598658867912,21.1013735009366));
#1428=CARTESIAN_POINT('Ctrl Pts',(0.7596584103706,-30.8465909355752,20.8721694081605));
#1429=CARTESIAN_POINT('Ctrl Pts',(1.98433800521209,-30.3798149635844,20.7575670418755));
#1430=CARTESIAN_POINT('Ctrl Pts',(3.52578602540974,-28.5931135200025,20.5283676296524));
#1431=CARTESIAN_POINT('Ctrl Pts',(3.8208190800791,-27.3005795704328,20.4137635916772));
#1432=CARTESIAN_POINT('Ctrl Pts',(3.18340034511317,-25.0004020130352,20.1845686868986));
#1433=CARTESIAN_POINT('Ctrl Pts',(2.26172892311522,-24.0264166801336,20.0699630275308));
#1434=CARTESIAN_POINT('Ctrl Pts',(-0.0310075805132356,-23.2709470686081,
19.840772464982));
#1435=CARTESIAN_POINT('Ctrl Pts',(-1.36774615552683,-23.4993356660845,19.7261652328664));
#1436=CARTESIAN_POINT('Ctrl Pts',(-3.29044999554861,-25.003443698954,19.4969788547815));
#1437=CARTESIAN_POINT('Ctrl Pts',(-3.84882652597964,-26.255889878113,19.3823700969656));
#1438=CARTESIAN_POINT('Ctrl Pts',(-3.66341653596594,-28.7171925636406,19.1531877526223));
#1439=CARTESIAN_POINT('Ctrl Pts',(-2.92366288113256,-29.8898022514147,19.0385775146034));
#1440=CARTESIAN_POINT('Ctrl Pts',(-0.750050065449063,-31.1155888685023,
18.8093990599493));
#1441=CARTESIAN_POINT('Ctrl Pts',(0.651110587682156,-31.1517796318851,18.6947873857344));
#1442=CARTESIAN_POINT('Ctrl Pts',(2.90172211077653,-30.0124147872479,18.4656126830036));
#1443=CARTESIAN_POINT('Ctrl Pts',(3.71853772096227,-28.8547645355866,18.3509996151738));
#1444=CARTESIAN_POINT('Ctrl Pts',(4.02392234264642,-26.3233804905586,18.1218285325501));
#1445=CARTESIAN_POINT('Ctrl Pts',(3.50918503257104,-24.9871031169595,18.0072141122992));
#1446=CARTESIAN_POINT('Ctrl Pts',(1.55288051607053,-23.3098136929698,17.7780465236243));
#1447=CARTESIAN_POINT('Ctrl Pts',(0.140896517323791,-22.9926200323223,17.6634307908027));
#1448=CARTESIAN_POINT('Ctrl Pts',(-2.36650964254058,-23.6955465860942,17.4342665752667));
#1449=CARTESIAN_POINT('Ctrl Pts',(-3.42532249325332,-24.7042160076948,17.319649568463));
#1450=CARTESIAN_POINT('Ctrl Pts',(-4.24151789226149,-27.205672166438,17.0904886102752));
#1451=CARTESIAN_POINT('Ctrl Pts',(-3.98794903777075,-28.6613021650618,16.9758703668355));
#1452=CARTESIAN_POINT('Ctrl Pts',(-2.34405122024042,-30.7505189403242,16.7467125550671));
#1453=CARTESIAN_POINT('Ctrl Pts',(-0.978754765971974,-31.3540484715026,
16.6320931111307));
#1454=CARTESIAN_POINT('Ctrl Pts',(1.02933886603348,-31.1972354808515,16.460227032321));
#1455=CARTESIAN_POINT('Ctrl Pts',(1.68709482472537,-30.9779968406706,16.4029168679907));
#1456=CARTESIAN_POINT('Ctrl Pts',(2.8240837151474,-30.2508925065775,16.2883402228593));
#1457=CARTESIAN_POINT('Ctrl Pts',(3.30314935266293,-29.7448544918448,16.2310297714992));
#1458=CARTESIAN_POINT('Ctrl Pts',(3.96627580118359,-28.5616040731508,16.116453854622));
#1459=CARTESIAN_POINT('Ctrl Pts',(4.15104388235541,-27.8860791480164,16.0591431204344));
#1460=CARTESIAN_POINT('Ctrl Pts',(4.17802239058402,-26.5231491652539,15.9445679195579));
#1461=CARTESIAN_POINT('Ctrl Pts',(4.02164463287101,-25.836899273559,15.8872569066736));
#1462=CARTESIAN_POINT('Ctrl Pts',(3.39969277305442,-24.6162176795914,15.7726824098211));
#1463=CARTESIAN_POINT('Ctrl Pts',(2.9359020278153,-24.0821430128742,15.7153711223063));
#1464=CARTESIAN_POINT('Ctrl Pts',(1.80627259289743,-23.295059368917,15.6007973177115));
#1465=CARTESIAN_POINT('Ctrl Pts',(1.14217129355625,-23.0415308728188,15.5434857595736));
#1466=CARTESIAN_POINT('Ctrl Pts',(-0.231877317222814,-22.8792861228552,
15.4289126357253));
#1467=CARTESIAN_POINT('Ctrl Pts',(-0.940537550161687,-22.9692999005262,
15.3716008109));
#1468=CARTESIAN_POINT('Ctrl Pts',(-2.23508230276584,-23.4765970744679,15.2570283565139));
#1469=CARTESIAN_POINT('Ctrl Pts',(-2.82042721228882,-23.8921601369938,15.1997162688729));
#1470=CARTESIAN_POINT('Ctrl Pts',(-3.72724254909164,-24.9550994865649,15.0851444728953));
#1471=CARTESIAN_POINT('Ctrl Pts',(-4.04904226418634,-25.6007082903028,15.0278321262568));
#1472=CARTESIAN_POINT('Ctrl Pts',(-4.34898179372202,-26.9722920315092,14.913260977831));
#1473=CARTESIAN_POINT('Ctrl Pts',(-4.32823823833014,-27.696864249156,14.8559483759565));
#1474=CARTESIAN_POINT('Ctrl Pts',(-3.94416673686108,-29.0543767984046,14.741377864454));
#1475=CARTESIAN_POINT('Ctrl Pts',(-3.58247834736109,-29.6866038630478,14.684065011041));
#1476=CARTESIAN_POINT('Ctrl Pts',(-2.59897553580158,-30.7075411869121,14.5694951260371));
#1477=CARTESIAN_POINT('Ctrl Pts',(-1.97893887953295,-31.0963900092535,14.5121820247212));
#1478=CARTESIAN_POINT('Ctrl Pts',(-0.62377058727827,-31.5350735702099,14.3976127560067));
#1479=CARTESIAN_POINT('Ctrl Pts',(0.109859887125028,-31.5858618602476,14.3402994103674));
#1480=CARTESIAN_POINT('Ctrl Pts',(1.51846868411767,-31.3325375520331,14.2257307479178));
#1481=CARTESIAN_POINT('Ctrl Pts',(2.19257064211805,-31.0299670824768,14.1684171614822));
#1482=CARTESIAN_POINT('Ctrl Pts',(3.32065975230898,-30.1381775844584,14.0538490954731));
#1483=CARTESIAN_POINT('Ctrl Pts',(3.77459621319051,-29.5507269915758,13.9965352717156));
#1484=CARTESIAN_POINT('Ctrl Pts',(4.35164549000208,-28.2261503388289,13.8819677925012));
#1485=CARTESIAN_POINT('Ctrl Pts',(4.47554085920862,-27.4906059318028,13.8246537348364));
#1486=CARTESIAN_POINT('Ctrl Pts',(4.35932633846837,-26.043646007592,13.7100868329779));
#1487=CARTESIAN_POINT('Ctrl Pts',(4.1206457473642,-25.3332578752253,13.6527725447744));
#1488=CARTESIAN_POINT('Ctrl Pts',(3.33223129728641,-24.106308328171,13.5382062109767));
#1489=CARTESIAN_POINT('Ctrl Pts',(2.78423731477771,-23.5899834651597,13.4808916955503));
#1490=CARTESIAN_POINT('Ctrl Pts',(1.50450674316234,-22.8764080003258,13.3663259207328));
#1491=CARTESIAN_POINT('Ctrl Pts',(0.774413779611081,-22.6785518889991,13.309011181339));
#1492=CARTESIAN_POINT('Ctrl Pts',(-0.69739330426496,-22.6525522223851,13.1944459565731));
#1493=CARTESIAN_POINT('Ctrl Pts',(-1.43794247925327,-22.8231062186778,13.1371309964266));
#1494=CARTESIAN_POINT('Ctrl Pts',(-2.7541948376007,-23.4972409646481,13.0225663129528));
#1495=CARTESIAN_POINT('Ctrl Pts',(-3.32948087019843,-23.9991290609593,12.9652511352145));
#1496=CARTESIAN_POINT('Ctrl Pts',(-4.17626345911414,-25.2198325829076,12.8506869844455));
#1497=CARTESIAN_POINT('Ctrl Pts',(-4.4481843446811,-25.936961310921,12.7933715922294));
#1498=CARTESIAN_POINT('Ctrl Pts',(-4.62015665278908,-27.4194785452993,12.6788079657272));
#1499=CARTESIAN_POINT('Ctrl Pts',(-4.52137115313415,-28.183579240772,12.621492362104));
#1500=CARTESIAN_POINT('Ctrl Pts',(-3.97152663554103,-29.5783806208201,12.5069292515898));
#1501=CARTESIAN_POINT('Ctrl Pts',(-3.5220951227733,-30.2084906103522,12.4496134395774));
#1502=CARTESIAN_POINT('Ctrl Pts',(-2.37437165907619,-31.183679244984,12.3350508369351));
#1503=CARTESIAN_POINT('Ctrl Pts',(-1.67779038310627,-31.5289988293348,12.277734819509));
#1504=CARTESIAN_POINT('Ctrl Pts',(-0.199197333900588,-31.8492812709321,
12.1631727167557));
#1505=CARTESIAN_POINT('Ctrl Pts',(0.581419535730091,-31.825256919753,12.1058564968451));
#1506=CARTESIAN_POINT('Ctrl Pts',(2.04290487097247,-31.4086885823989,11.9912948861633));
#1507=CARTESIAN_POINT('Ctrl Pts',(2.72301785637377,-31.017689933097,11.9339784666505));
#1508=CARTESIAN_POINT('Ctrl Pts',(3.82034316796606,-29.9565159886648,11.8194173403514));
#1509=CARTESIAN_POINT('Ctrl Pts',(4.23761275995296,-29.2880562452814,11.7621007240815));
#1510=CARTESIAN_POINT('Ctrl Pts',(4.70706068115205,-27.8283747226536,11.6475400746183));
#1511=CARTESIAN_POINT('Ctrl Pts',(4.76009229327592,-27.0386382546772,11.5902232643864));
#1512=CARTESIAN_POINT('Ctrl Pts',(4.48463927434238,-25.5233462828554,11.4756630843606));
#1513=CARTESIAN_POINT('Ctrl Pts',(4.15760185288866,-24.7987006850272,11.4183460829245));
#1514=CARTESIAN_POINT('Ctrl Pts',(3.19600835697949,-23.5869462478655,11.3037863650511));
#1515=CARTESIAN_POINT('Ctrl Pts',(2.56315379146772,-23.099962191222,11.2464691751292));
#1516=CARTESIAN_POINT('Ctrl Pts',(1.13757263913847,-22.4820219779078,11.1319099122695));
#1517=CARTESIAN_POINT('Ctrl Pts',(0.346404347142174,-22.3503795041057,11.0745925365344));
#1518=CARTESIAN_POINT('Ctrl Pts',(-1.76387591167285,-22.5237230755283,10.9191576492385));
#1519=CARTESIAN_POINT('Ctrl Pts',(-3.04213419140331,-23.2249589278969,10.8209586709532));
#1520=CARTESIAN_POINT('Ctrl Pts',(-4.26287386638314,-24.8351878142477,10.6736877485838));
#1521=CARTESIAN_POINT('Ctrl Pts',(-4.55417709738229,-25.4602183705301,10.6246080237907));
#1522=CARTESIAN_POINT('Ctrl Pts',(-4.78298015330037,-26.4482305165422,10.5509677380958));
#1523=CARTESIAN_POINT('Ctrl Pts',(-4.82497450026767,-26.7858033043513,10.5264227857054));
#1524=CARTESIAN_POINT('Ctrl Pts',(-4.83612470074125,-27.4630368812996,10.4773448839533));
#1525=CARTESIAN_POINT('Ctrl Pts',(-4.81152195248019,-27.8040996825675,10.4527957512917));
#1526=CARTESIAN_POINT('Ctrl Pts',(-4.7966595069499,-28.1445096413087,10.4282516293878));
#1527=CARTESIAN_POINT('Ctrl Pts',(-2.50007468503219,-27.1253399927944,21.5012668209833));
#1528=CARTESIAN_POINT('Ctrl Pts',(-2.51283639211379,-27.5313396040275,21.4450628827391));
#1529=CARTESIAN_POINT('Ctrl Pts',(-2.42258993385229,-27.9512582892639,21.3862340567569));
#1530=CARTESIAN_POINT('Ctrl Pts',(-1.87705908045303,-29.0525304994187,21.2178402639005));
#1531=CARTESIAN_POINT('Ctrl Pts',(-1.11370965992309,-29.6026650811217,21.1000517830227));
#1532=CARTESIAN_POINT('Ctrl Pts',(0.538323541218874,-29.815954615602,20.8754777398045));
#1533=CARTESIAN_POINT('Ctrl Pts',(1.43377361752959,-29.4808752026413,20.7577246144251));
#1534=CARTESIAN_POINT('Ctrl Pts',(2.54587760682549,-28.2045638431909,20.5331025971331));
#1535=CARTESIAN_POINT('Ctrl Pts',(2.76750114097136,-27.2589325509883,20.4153840366144));
#1536=CARTESIAN_POINT('Ctrl Pts',(2.31593508025811,-25.5993026196536,20.1907150274047));
#1537=CARTESIAN_POINT('Ctrl Pts',(1.6419110691535,-24.8790793164352,20.0730302677181));
#1538=CARTESIAN_POINT('Ctrl Pts',(-0.0149683894611636,-24.3249408654976,
19.8483152194252));
#1539=CARTESIAN_POINT('Ctrl Pts',(-1.00313453278291,-24.4884039772537,19.7306635219149));
#1540=CARTESIAN_POINT('Ctrl Pts',(-2.4051781686742,-25.5756604965874,19.5059033598245));
#1541=CARTESIAN_POINT('Ctrl Pts',(-2.82388459307759,-26.5022176830049,19.3882840101185));
#1542=CARTESIAN_POINT('Ctrl Pts',(-2.69582100380578,-28.2990165041629,19.1634796322399));
#1543=CARTESIAN_POINT('Ctrl Pts',(-2.14943180799116,-29.1744485529642,19.0458919391655));
#1544=CARTESIAN_POINT('Ctrl Pts',(-0.560198814082305,-30.0787479984767,
18.8210442180266));
#1545=CARTESIAN_POINT('Ctrl Pts',(0.486450458466467,-30.1106125532363,18.7034875125573));
#1546=CARTESIAN_POINT('Ctrl Pts',(2.14509782251475,-29.2785424876867,18.478597295444));
#1547=CARTESIAN_POINT('Ctrl Pts',(2.76136687700576,-28.4132455801264,18.3610709299044));
#1548=CARTESIAN_POINT('Ctrl Pts',(2.99339233231008,-26.5447839295675,18.1361390401663));
#1549=CARTESIAN_POINT('Ctrl Pts',(2.61031700332953,-25.5376669816206,18.0186423872216));
#1550=CARTESIAN_POINT('Ctrl Pts',(1.16446086543928,-24.2896610973114,17.7936696249626));
#1551=CARTESIAN_POINT('Ctrl Pts',(0.09930017734222,-24.0458624466996,17.6762020766647));
#1552=CARTESIAN_POINT('Ctrl Pts',(-1.7675888393034,-24.5628529769143,17.4511892199568));
#1553=CARTESIAN_POINT('Ctrl Pts',(-2.57270112799042,-25.3239325128253,17.333750187231));
#1554=CARTESIAN_POINT('Ctrl Pts',(-3.18765925209663,-27.1895201174977,17.1086979919401));
#1555=CARTESIAN_POINT('Ctrl Pts',(-2.99900529386622,-28.296664824665,16.991286903718));
#1556=CARTESIAN_POINT('Ctrl Pts',(-1.77201713798893,-29.8653042054102,16.7661961054407));
#1557=CARTESIAN_POINT('Ctrl Pts',(-0.732529681096322,-30.3292078520877,
16.6488124076455));
#1558=CARTESIAN_POINT('Ctrl Pts',(0.777221611436293,-30.2154776693097,16.4799658932922));
#1559=CARTESIAN_POINT('Ctrl Pts',(1.28140778933044,-30.049082741554,16.4212841687898));
#1560=CARTESIAN_POINT('Ctrl Pts',(2.13894102609193,-29.5039217906006,16.3087104851517));
#1561=CARTESIAN_POINT('Ctrl Pts',(2.50748319588252,-29.1168780348298,16.2500354076075));
#1562=CARTESIAN_POINT('Ctrl Pts',(3.00992376655387,-28.2258212672248,16.1374524690789));
#1563=CARTESIAN_POINT('Ctrl Pts',(3.15331377168557,-27.7073372554579,16.0787839738266));
#1564=CARTESIAN_POINT('Ctrl Pts',(3.17632285443344,-26.6778431099855,15.9661918649761));
#1565=CARTESIAN_POINT('Ctrl Pts',(3.05748130255417,-26.1495930224966,15.9075298882322));
#1566=CARTESIAN_POINT('Ctrl Pts',(2.58921125566468,-25.2248424296844,15.7949286927493));
#1567=CARTESIAN_POINT('Ctrl Pts',(2.2330033354922,-24.8124137254194,15.7362731716848));
#1568=CARTESIAN_POINT('Ctrl Pts',(1.37840967612313,-24.2138679666298,15.6236629718413));
#1569=CARTESIAN_POINT('Ctrl Pts',(0.866528503509928,-24.0169055865723,15.5650138445848));
#1570=CARTESIAN_POINT('Ctrl Pts',(-0.176086822448727,-23.8912812923305,
15.4523947217693));
#1571=CARTESIAN_POINT('Ctrl Pts',(-0.723839333138843,-23.9594255922406,
15.3937519273021));
#1572=CARTESIAN_POINT('Ctrl Pts',(-1.70882778077597,-24.342780211676,15.2811239616996));
#1573=CARTESIAN_POINT('Ctrl Pts',(-2.16257723397831,-24.6632061601177,15.2224874398782));
#1574=CARTESIAN_POINT('Ctrl Pts',(-2.85481959844414,-25.4709142401168,15.1098507107457));
#1575=CARTESIAN_POINT('Ctrl Pts',(-3.10541208162622,-25.9705887465318,15.0512204022701));
#1576=CARTESIAN_POINT('Ctrl Pts',(-3.33643491243401,-27.0159322908697,14.9385749877282));
#1577=CARTESIAN_POINT('Ctrl Pts',(-3.3216858471879,-27.578238681535,14.8799508342142));
#1578=CARTESIAN_POINT('Ctrl Pts',(-3.03062657946405,-28.6155506117409,14.7672968113139));
#1579=CARTESIAN_POINT('Ctrl Pts',(-2.75071538543883,-29.1075013221103,14.7086787551844));
#1580=CARTESIAN_POINT('Ctrl Pts',(-2.00018375681689,-29.8898980947296,14.5960162000601));
#1581=CARTESIAN_POINT('Ctrl Pts',(-1.51839135128136,-30.1935863948407,14.5374041844901));
#1582=CARTESIAN_POINT('Ctrl Pts',(-0.481129998089667,-30.5317228493949,
14.4247331723202));
#1583=CARTESIAN_POINT('Ctrl Pts',(0.0904391347614876,-30.5725753124629,
14.3661271413499));
#1584=CARTESIAN_POINT('Ctrl Pts',(1.17128619067979,-30.3804399078241,14.2534477461713));
#1585=CARTESIAN_POINT('Ctrl Pts',(1.69778284783799,-30.1455013508672,14.1948476446037));
#1586=CARTESIAN_POINT('Ctrl Pts',(2.56566196202055,-29.4621820446215,14.0821599397072));
#1587=CARTESIAN_POINT('Ctrl Pts',(2.9213066794093,-29.0039557713287,14.0235657131016));
#1588=CARTESIAN_POINT('Ctrl Pts',(3.36714885804308,-27.9858932409967,13.9108697706508));
#1589=CARTESIAN_POINT('Ctrl Pts',(3.46527617925812,-27.4106453730656,13.8522813653494));
#1590=CARTESIAN_POINT('Ctrl Pts',(3.37784082869232,-26.295852639153,13.7395772567127));
#1591=CARTESIAN_POINT('Ctrl Pts',(3.19199787774012,-25.7389764859617,13.6809946198038));
#1592=CARTESIAN_POINT('Ctrl Pts',(2.58554795284393,-24.7913997988873,13.5682824152982));
#1593=CARTESIAN_POINT('Ctrl Pts',(2.15651559470711,-24.3855495363483,13.5097054945602));
#1594=CARTESIAN_POINT('Ctrl Pts',(1.16895684306617,-23.832575565039,13.3969852638233));
#1595=CARTESIAN_POINT('Ctrl Pts',(0.595852596233928,-23.6760691824297,13.3384140077367));
#1596=CARTESIAN_POINT('Ctrl Pts',(-0.542579588650037,-23.6539742782162,
13.225685819334));
#1597=CARTESIAN_POINT('Ctrl Pts',(-1.1251889792854,-23.7869913050767,13.1671201771495));
#1598=CARTESIAN_POINT('Ctrl Pts',(-2.14559645901048,-24.3074163661573,13.054384098833));
#1599=CARTESIAN_POINT('Ctrl Pts',(-2.59929053184396,-24.7017492310162,12.9958240204473));
#1600=CARTESIAN_POINT('Ctrl Pts',(-3.25762576760017,-25.647434253134,12.8830801191498));
#1601=CARTESIAN_POINT('Ctrl Pts',(-3.47301577972443,-26.2123929560692,12.824525555112));
#1602=CARTESIAN_POINT('Ctrl Pts',(-3.60843998708556,-27.363536579556,12.7117738969421));
#1603=CARTESIAN_POINT('Ctrl Pts',(-3.53153182161548,-27.9667909104199,12.6532247984982));
#1604=CARTESIAN_POINT('Ctrl Pts',(-3.10566528390168,-29.0521245514136,12.5404654486599));
#1605=CARTESIAN_POINT('Ctrl Pts',(-2.75134896750393,-29.5506975660807,12.4819217677002));
#1606=CARTESIAN_POINT('Ctrl Pts',(-1.85884518892285,-30.3114094990717,12.369154790682));
#1607=CARTESIAN_POINT('Ctrl Pts',(-1.30815106795505,-30.5855637052752,12.3106164797331));
#1608=CARTESIAN_POINT('Ctrl Pts',(-0.155741001580881,-30.8370096520725,
12.1978419391373));
#1609=CARTESIAN_POINT('Ctrl Pts',(0.462671842753837,-30.8189948910673,12.1393089513662));
#1610=CARTESIAN_POINT('Ctrl Pts',(1.60404657876531,-30.4954824535707,12.0265269100757));
#1611=CARTESIAN_POINT('Ctrl Pts',(2.14394545222966,-30.1862453058223,11.9679991992472));
#1612=CARTESIAN_POINT('Ctrl Pts',(3.0028316585045,-29.3580377153228,11.8552097193461));
#1613=CARTESIAN_POINT('Ctrl Pts',(3.33498881469216,-28.8277788561896,11.7966872398373));
#1614=CARTESIAN_POINT('Ctrl Pts',(3.70397767040327,-27.685950722295,11.6838903826651));
#1615=CARTESIAN_POINT('Ctrl Pts',(3.74709584473805,-27.0582142459975,11.6253730894484));
#1616=CARTESIAN_POINT('Ctrl Pts',(3.5328841786163,-25.8705936164613,11.5125689155825));
#1617=CARTESIAN_POINT('Ctrl Pts',(3.2734696560962,-25.2934880851587,11.4540567642246));
#1618=CARTESIAN_POINT('Ctrl Pts',(2.520349254524,-24.3418377285451,11.3412453335038));
#1619=CARTESIAN_POINT('Ctrl Pts',(2.01668017794548,-23.9530915623133,11.2827382801346));
#1620=CARTESIAN_POINT('Ctrl Pts',(0.897564453532843,-23.4662627472373,11.1699196516999));
#1621=CARTESIAN_POINT('Ctrl Pts',(0.266632689637674,-23.3603587008251,11.111417653014));
#1622=CARTESIAN_POINT('Ctrl Pts',(-1.39308043271686,-23.4945707094314,10.9583341865454));
#1623=CARTESIAN_POINT('Ctrl Pts',(-2.41051507768367,-24.0480090686017,10.8592926132578));
#1624=CARTESIAN_POINT('Ctrl Pts',(-3.38001927688757,-25.3235976874956,10.712152032226));
#1625=CARTESIAN_POINT('Ctrl Pts',(-3.61034539690739,-25.8164734424502,10.6637184246244));
#1626=CARTESIAN_POINT('Ctrl Pts',(-3.7931173904721,-26.6014371673577,10.589901366163));
#1627=CARTESIAN_POINT('Ctrl Pts',(-3.82668517274698,-26.8694485711687,10.565370259987));
#1628=CARTESIAN_POINT('Ctrl Pts',(-3.83611228951587,-27.4039358312353,10.517059613737));
#1629=CARTESIAN_POINT('Ctrl Pts',(-3.81313732847822,-27.7633656624966,10.4924048684869));
#1630=CARTESIAN_POINT('Ctrl Pts',(-3.79827488294779,-28.1037756212366,10.4678607465822));
#1631=CARTESIAN_POINT('Ctrl Pts',(-2.50007468503219,-27.2248833652324,22.4963000450535));
#1632=CARTESIAN_POINT('Ctrl Pts',(-2.4973230516022,-27.6307229864326,22.4401121123047));
#1633=CARTESIAN_POINT('Ctrl Pts',(-2.3900690404148,-28.0461795533903,22.3813056708375));
#1634=CARTESIAN_POINT('Ctrl Pts',(-1.80410662012797,-29.1255019961691,22.2129753102057));
#1635=CARTESIAN_POINT('Ctrl Pts',(-1.01989116822409,-29.6445438741314,22.0952214478198));
#1636=CARTESIAN_POINT('Ctrl Pts',(0.638667716265594,-29.7975756887231,21.8707222568133));
#1637=CARTESIAN_POINT('Ctrl Pts',(1.52050852311385,-29.42808298243,21.7530071973406));
#1638=CARTESIAN_POINT('Ctrl Pts',(2.58730699957112,-28.1125682867517,21.5284506711618));
#1639=CARTESIAN_POINT('Ctrl Pts',(2.77328137790538,-27.1587131575376,21.4107735199278));
#1640=CARTESIAN_POINT('Ctrl Pts',(2.26433740680624,-25.5138475614163,21.1861609869398));
#1641=CARTESIAN_POINT('Ctrl Pts',(1.56360921374272,-24.8180370750652,21.0685208793189));
#1642=CARTESIAN_POINT('Ctrl Pts',(-0.113585913522054,-24.3188787500937,
20.8438536227986));
#1643=CARTESIAN_POINT('Ctrl Pts',(-1.09686428893776,-24.5178009465808,20.7262497228448));
#1644=CARTESIAN_POINT('Ctrl Pts',(-2.46563320123022,-25.6525768382252,20.5015289835988));
#1645=CARTESIAN_POINT('Ctrl Pts',(-2.85270548558921,-26.5950753813576,20.3839604828611));
#1646=CARTESIAN_POINT('Ctrl Pts',(-2.66720295546915,-28.3916002393823,20.1591874603215));
#1647=CARTESIAN_POINT('Ctrl Pts',(-2.09003931759816,-29.2502156366228,20.0416535766241));
#1648=CARTESIAN_POINT('Ctrl Pts',(-0.468609715717802,-30.1076026169081,
19.8168294314625));
#1649=CARTESIAN_POINT('Ctrl Pts',(0.581641933078928,-30.1049235048463,19.6993294077519));
#1650=CARTESIAN_POINT('Ctrl Pts',(2.22027058723989,-29.2201403231244,19.4744552627731));
#1651=CARTESIAN_POINT('Ctrl Pts',(2.81040201556557,-28.3324660884538,19.3569883662253));
#1652=CARTESIAN_POINT('Ctrl Pts',(2.98817347828617,-26.4505240261162,19.1320653083975));
#1653=CARTESIAN_POINT('Ctrl Pts',(2.57213067357672,-25.4521246224307,19.0146308292871));
#1654=CARTESIAN_POINT('Ctrl Pts',(1.08461238202261,-24.2407098526991,18.7896599110507));
#1655=CARTESIAN_POINT('Ctrl Pts',(0.00799178041480618,-24.0287177017401,
18.6722571617048));
#1656=CARTESIAN_POINT('Ctrl Pts',(-1.85263633527269,-24.6003741985188,18.4472394027778));
#1657=CARTESIAN_POINT('Ctrl Pts',(-2.63825121549225,-25.388732377058,18.3298677169699));
#1658=CARTESIAN_POINT('Ctrl Pts',(-3.205081356731,-27.2801569719116,18.1048041047243));
#1659=CARTESIAN_POINT('Ctrl Pts',(-2.9831649376875,-28.3867672345334,17.9874628367108));
#1660=CARTESIAN_POINT('Ctrl Pts',(-1.70783979269738,-29.9307710004345,17.7623543286427));
#1661=CARTESIAN_POINT('Ctrl Pts',(-0.650024237860058,-30.3672113434981,
17.6450428520577));
#1662=CARTESIAN_POINT('Ctrl Pts',(0.865186630000211,-30.2134208155298,17.4761784953134));
#1663=CARTESIAN_POINT('Ctrl Pts',(1.36725623215089,-30.0318398410671,17.4175337661475));
#1664=CARTESIAN_POINT('Ctrl Pts',(2.21566236248619,-29.4614040789813,17.304946706094));
#1665=CARTESIAN_POINT('Ctrl Pts',(2.57530571424416,-29.0619405854776,17.2463091979379));
#1666=CARTESIAN_POINT('Ctrl Pts',(3.05800073394719,-28.1527721613655,17.1337114265062));
#1667=CARTESIAN_POINT('Ctrl Pts',(3.1877871455815,-27.6274487856325,17.0750810662931));
#1668=CARTESIAN_POINT('Ctrl Pts',(3.18497727452253,-26.5910785688795,16.9624726925251));
#1669=CARTESIAN_POINT('Ctrl Pts',(3.05096295225393,-26.0630919115944,16.9038494082137));
#1670=CARTESIAN_POINT('Ctrl Pts',(2.55669827095366,-25.144200958879,16.7912305397785));
#1671=CARTESIAN_POINT('Ctrl Pts',(2.18722058458361,-24.7390313387568,16.732614260404));
#1672=CARTESIAN_POINT('Ctrl Pts',(1.31236252412446,-24.1576827525991,16.6199850030865));
#1673=CARTESIAN_POINT('Ctrl Pts',(0.792130109930538,-23.9732737150518,16.561375658774));
#1674=CARTESIAN_POINT('Ctrl Pts',(-0.260444433079681,-23.8722198598602,
16.4487361169824));
#1675=CARTESIAN_POINT('Ctrl Pts',(-0.809754840681111,-23.9553140876739,
16.3901336388362));
#1676=CARTESIAN_POINT('Ctrl Pts',(-1.79218414638217,-24.3649938942232,16.2774839153377));
#1677=CARTESIAN_POINT('Ctrl Pts',(-2.24038399479556,-24.6993401595432,16.2188882354581));
#1678=CARTESIAN_POINT('Ctrl Pts',(-2.91818815440847,-25.529137615882,16.1062284316294));
#1679=CARTESIAN_POINT('Ctrl Pts',(-3.15743206857856,-26.0385320297141,16.0476394830881));
#1680=CARTESIAN_POINT('Ctrl Pts',(-3.3654714364124,-27.0967271438523,15.9349696987346));
#1681=CARTESIAN_POINT('Ctrl Pts',(-3.33619825815045,-27.662358669908,15.8763874156349));
#1682=CARTESIAN_POINT('Ctrl Pts',(-3.01887060851525,-28.7004015301552,15.7637077490722));
#1683=CARTESIAN_POINT('Ctrl Pts',(-2.72459263582721,-29.188559158675,15.7051320664418));
#1684=CARTESIAN_POINT('Ctrl Pts',(-1.9504930567998,-29.9594480905514,15.5924426146465));
#1685=CARTESIAN_POINT('Ctrl Pts',(-1.45776997299186,-30.2531292770361,15.5338734683806));
#1686=CARTESIAN_POINT('Ctrl Pts',(-0.404990234426755,-30.5701818753113,
15.4211743269738));
#1687=CARTESIAN_POINT('Ctrl Pts',(0.171595902055322,-30.5971301657918,15.3626116539469));
#1688=CARTESIAN_POINT('Ctrl Pts',(1.25641083541538,-30.379164019775,15.2499029170041));
#1689=CARTESIAN_POINT('Ctrl Pts',(1.78089508984846,-30.1296184738905,15.1913466549704));
#1690=CARTESIAN_POINT('Ctrl Pts',(2.64032744040503,-29.4216132578738,15.07862841543));
#1691=CARTESIAN_POINT('Ctrl Pts',(2.98742402928102,-28.951416043259,15.0200785030053));
#1692=CARTESIAN_POINT('Ctrl Pts',(3.41436537442326,-27.9154253975122,14.9073508523134));
#1693=CARTESIAN_POINT('Ctrl Pts',(3.49939161592954,-27.3335641004151,14.8488072290052));
#1694=CARTESIAN_POINT('Ctrl Pts',(3.38693299773095,-26.2116611333541,14.7360702574282));
#1695=CARTESIAN_POINT('Ctrl Pts',(3.18644882156979,-25.6550153663941,14.6775328635923));
#1696=CARTESIAN_POINT('Ctrl Pts',(2.5545653302512,-24.712735350079,14.5647866600073));
#1697=CARTESIAN_POINT('Ctrl Pts',(2.11270270631046,-24.3138769369602,14.5062554367953));
#1698=CARTESIAN_POINT('Ctrl Pts',(1.10509122951777,-23.7773695884842,14.3935000890219));
#1699=CARTESIAN_POINT('Ctrl Pts',(0.523891228402976,-23.6329909911365,14.3349749783932));
#1700=CARTESIAN_POINT('Ctrl Pts',(-0.624659171511437,-23.6347573525544,
14.2222105728532));
#1701=CARTESIAN_POINT('Ctrl Pts',(-1.20879903018357,-23.7822465505066,14.1636915176313));
#1702=CARTESIAN_POINT('Ctrl Pts',(-2.22710672018521,-24.328477425712,14.0509181395924));
#1703=CARTESIAN_POINT('Ctrl Pts',(-2.67544143431689,-24.7363107813614,13.99240508335));
#1704=CARTESIAN_POINT('Ctrl Pts',(-3.31996060297977,-25.7038637739138,13.879622816927));
#1705=CARTESIAN_POINT('Ctrl Pts',(-3.52435156498093,-26.2782694012189,13.821115703984));
#1706=CARTESIAN_POINT('Ctrl Pts',(-3.63741165163986,-27.4423671822191,13.7083246321569));
#1707=CARTESIAN_POINT('Ctrl Pts',(-3.54639862955187,-28.0488697379073,13.6498234076231));
#1708=CARTESIAN_POINT('Ctrl Pts',(-3.09472995624812,-29.1353049846404,13.5370236121474));
#1709=CARTESIAN_POINT('Ctrl Pts',(-2.72643785221591,-29.6302056579101,13.4785282218764));
#1710=CARTESIAN_POINT('Ctrl Pts',(-1.81058044300674,-30.3799313917062,13.3657197834808));
#1711=CARTESIAN_POINT('Ctrl Pts',(-1.24923466426418,-30.6443543382562,13.3072301740502));
#1712=CARTESIAN_POINT('Ctrl Pts',(-0.0812416818551773,-30.8752452508522,
13.1944131722907));
#1713=CARTESIAN_POINT('Ctrl Pts',(0.542072912261212,-30.8436839153864,13.1359292910085));
#1714=CARTESIAN_POINT('Ctrl Pts',(1.68771332512077,-30.4947449192179,13.0231038044166));
#1715=CARTESIAN_POINT('Ctrl Pts',(2.22565936133885,-30.1712550743319,12.9646255992779));
#1716=CARTESIAN_POINT('Ctrl Pts',(3.07652976944644,-29.3185537876298,12.8517917053114));
#1717=CARTESIAN_POINT('Ctrl Pts',(3.40034470317039,-28.7765983337464,12.7933191250111));
#1718=CARTESIAN_POINT('Ctrl Pts',(3.75087283940905,-27.6167979591164,12.6804769000917));
#1719=CARTESIAN_POINT('Ctrl Pts',(3.78118424110462,-26.9825905474799,12.6220098940059));
#1720=CARTESIAN_POINT('Ctrl Pts',(3.54228501118274,-25.7876184262315,12.5091594135308));
#1721=CARTESIAN_POINT('Ctrl Pts',(3.26854034758218,-25.2107358862553,12.4506979317093));
#1722=CARTESIAN_POINT('Ctrl Pts',(2.49014343782273,-24.2640304588299,12.337839270068));
#1723=CARTESIAN_POINT('Ctrl Pts',(1.97390393644558,-23.8821352485647,12.2793832632066));
#1724=CARTESIAN_POINT('Ctrl Pts',(0.834695096751776,-23.4114174957062,12.1665164938306));
#1725=CARTESIAN_POINT('Ctrl Pts',(0.195826419298673,-23.3174103743359,12.108065913277));
#1726=CARTESIAN_POINT('Ctrl Pts',(-1.47788831221255,-23.4836403788777,11.9549159128501));
#1727=CARTESIAN_POINT('Ctrl Pts',(-2.49444407803175,-24.0624268927996,11.8559193209146));
#1728=CARTESIAN_POINT('Ctrl Pts',(-3.44927812351996,-25.3687964002138,11.7087911217838));
#1729=CARTESIAN_POINT('Ctrl Pts',(-3.67294914345905,-25.8708468387751,11.6603404761587));
#1730=CARTESIAN_POINT('Ctrl Pts',(-3.84264473622583,-26.6669563054752,11.5865392576738));
#1731=CARTESIAN_POINT('Ctrl Pts',(-3.87152605079722,-26.9382169121315,11.5620098124717));
#1732=CARTESIAN_POINT('Ctrl Pts',(-3.87149305127384,-27.4782945532475,11.5136784821176));
#1733=CARTESIAN_POINT('Ctrl Pts',(-3.84967986989137,-27.8368197194528,11.4890337583855));
#1734=CARTESIAN_POINT('Ctrl Pts',(-3.83481742436109,-28.1772296781916,11.4644896364825));
#1735=CARTESIAN_POINT('Ctrl Pts',(-3.5,-27.2127225901214,22.4975166120351));
#1736=CARTESIAN_POINT('Ctrl Pts',(-3.49927785868713,-27.7853287709716,22.4402329481162));
#1737=CARTESIAN_POINT('Ctrl Pts',(-3.35446180200001,-28.3588230843844,22.3829524737063));
#1738=CARTESIAN_POINT('Ctrl Pts',(-2.53808767932955,-29.8821237915549,22.2111091898206));
#1739=CARTESIAN_POINT('Ctrl Pts',(-1.46145231937317,-30.6017446798008,22.0965431657326));
#1740=CARTESIAN_POINT('Ctrl Pts',(0.860002585417323,-30.8282120086964,21.8674139251703));
#1741=CARTESIAN_POINT('Ctrl Pts',(2.07107291079633,-30.3270227433741,21.752849624791));
#1742=CARTESIAN_POINT('Ctrl Pts',(3.56721541815537,-28.5011179635623,21.5237157036811));
#1743=CARTESIAN_POINT('Ctrl Pts',(3.82659931701312,-27.20036017698,21.4091530749885));
#1744=CARTESIAN_POINT('Ctrl Pts',(3.13180267166131,-24.9149469548,21.1800146464357));
#1745=CARTESIAN_POINT('Ctrl Pts',(2.18342706770339,-23.9653744387647,21.0654536391327));
#1746=CARTESIAN_POINT('Ctrl Pts',(-0.129625104573071,-23.2648849532031,
20.8363108683544));
#1747=CARTESIAN_POINT('Ctrl Pts',(-1.46147591168062,-23.5287326354126,20.7217514337973));
#1748=CARTESIAN_POINT('Ctrl Pts',(-3.35090502810569,-25.0803600405907,20.4926044785548));
#1749=CARTESIAN_POINT('Ctrl Pts',(-3.87764741849126,-26.3487475764667,20.3780465697071));
#1750=CARTESIAN_POINT('Ctrl Pts',(-3.63479848762931,-28.8097762988588,20.148895580705));
#1751=CARTESIAN_POINT('Ctrl Pts',(-2.86427039073957,-29.9655693350743,20.0343391520621));
#1752=CARTESIAN_POINT('Ctrl Pts',(-0.65846096708456,-31.1444434869326,19.8051842733852));
#1753=CARTESIAN_POINT('Ctrl Pts',(0.74630206229462,-31.1460905834951,19.6906292809279));
#1754=CARTESIAN_POINT('Ctrl Pts',(2.97689487550167,-29.9540126226856,19.4614706503338));
#1755=CARTESIAN_POINT('Ctrl Pts',(3.76757285952208,-28.7739850439139,19.3469170514958));
#1756=CARTESIAN_POINT('Ctrl Pts',(4.0187034886225,-26.2291205871072,19.1177548007802));
#1757=CARTESIAN_POINT('Ctrl Pts',(3.47099870281935,-24.9015607577697,19.0032025543658));
#1758=CARTESIAN_POINT('Ctrl Pts',(1.47303203265274,-23.2608624483575,18.7740368097113));
#1759=CARTESIAN_POINT('Ctrl Pts',(0.0495881203952384,-22.9754752873616,
18.6594858758451));
#1760=CARTESIAN_POINT('Ctrl Pts',(-2.45155713850874,-23.7330678076998,18.4303167580854));
#1761=CARTESIAN_POINT('Ctrl Pts',(-3.49087258075457,-24.7690158719264,18.3157670982032));
#1762=CARTESIAN_POINT('Ctrl Pts',(-4.25893999689643,-27.296309020853,18.0865947230583));
#1763=CARTESIAN_POINT('Ctrl Pts',(-3.97210868158914,-28.7514045749302,17.9720462998272));
#1764=CARTESIAN_POINT('Ctrl Pts',(-2.27987387495177,-30.8159857353485,17.7428707782702));
#1765=CARTESIAN_POINT('Ctrl Pts',(-0.896249322735714,-31.3920519629118,
17.6283235555406));
#1766=CARTESIAN_POINT('Ctrl Pts',(1.11730388459739,-31.1951786270721,17.4564396343434));
#1767=CARTESIAN_POINT('Ctrl Pts',(1.77294326754581,-30.9607539401843,17.3991664653485));
#1768=CARTESIAN_POINT('Ctrl Pts',(2.90080505154166,-30.2083747949576,17.2845764438015));
#1769=CARTESIAN_POINT('Ctrl Pts',(3.37097187102428,-29.6899170424932,17.2273035618313));
#1770=CARTESIAN_POINT('Ctrl Pts',(4.01435276857721,-28.4885549672909,17.1127128120475));
#1771=CARTESIAN_POINT('Ctrl Pts',(4.18551725625119,-27.8061906781911,17.0554402129015));
#1772=CARTESIAN_POINT('Ctrl Pts',(4.18667681067326,-26.4363846241478,16.9408487471063));
#1773=CARTESIAN_POINT('Ctrl Pts',(4.01512628257138,-25.7503981626563,16.8835764266556));
#1774=CARTESIAN_POINT('Ctrl Pts',(3.3671797883428,-24.5355762087865,16.7689842568497));
#1775=CARTESIAN_POINT('Ctrl Pts',(2.89011927690729,-24.0087606262116,16.7117122110268));
#1776=CARTESIAN_POINT('Ctrl Pts',(1.74022544089816,-23.2388741548863,16.5971193489555));
#1777=CARTESIAN_POINT('Ctrl Pts',(1.06777289997686,-22.997899001297,16.5398475737628));
#1778=CARTESIAN_POINT('Ctrl Pts',(-0.316234927853767,-22.8602246903861,
16.4252540309383));
#1779=CARTESIAN_POINT('Ctrl Pts',(-1.02645305770396,-22.9651883959601,16.3679825224341));
#1780=CARTESIAN_POINT('Ctrl Pts',(-2.31843866837204,-23.4988107570144,16.253388310152));
#1781=CARTESIAN_POINT('Ctrl Pts',(-2.89823397310667,-23.9282941364198,16.196117064454));
#1782=CARTESIAN_POINT('Ctrl Pts',(-3.79061110505536,-25.0133228623296,16.0815221937778));
#1783=CARTESIAN_POINT('Ctrl Pts',(-4.10106225113868,-25.6686515734845,16.0242512070742));
#1784=CARTESIAN_POINT('Ctrl Pts',(-4.37801831770041,-27.0530868844925,15.909655688838));
#1785=CARTESIAN_POINT('Ctrl Pts',(-4.34275064929299,-27.7809842375283,15.8523849573772));
#1786=CARTESIAN_POINT('Ctrl Pts',(-3.93241076591198,-29.1392277168195,15.7377888022123));
#1787=CARTESIAN_POINT('Ctrl Pts',(-3.55635559774948,-29.7676616996119,15.6805183222975));
#1788=CARTESIAN_POINT('Ctrl Pts',(-2.5492848357845,-30.7770911827345,15.5659215406245));
#1789=CARTESIAN_POINT('Ctrl Pts',(-1.91831750124282,-31.1559328914483,15.508651308613));
#1790=CARTESIAN_POINT('Ctrl Pts',(-0.547630823615979,-31.573532596127,15.3940539106591));
#1791=CARTESIAN_POINT('Ctrl Pts',(0.191016654419482,-31.6104167135759,15.3367839229662));
#1792=CARTESIAN_POINT('Ctrl Pts',(1.60359332885263,-31.3312616639846,15.2221859187487));
#1793=CARTESIAN_POINT('Ctrl Pts',(2.27568288412789,-31.0140842055001,15.1649161718489));
#1794=CARTESIAN_POINT('Ctrl Pts',(3.39532523069409,-30.0976087977106,15.0503175711959));
#1795=CARTESIAN_POINT('Ctrl Pts',(3.84071356306253,-29.4981872635055,14.9930480616187));
#1796=CARTESIAN_POINT('Ctrl Pts',(4.39886200638194,-28.1556824953451,14.8784488741645));
#1797=CARTESIAN_POINT('Ctrl Pts',(4.50965629588013,-27.4135246591517,14.821179598491));
#1798=CARTESIAN_POINT('Ctrl Pts',(4.36841850750692,-25.9594545017938,14.7065798336947));
#1799=CARTESIAN_POINT('Ctrl Pts',(4.11509669119356,-25.2492967556584,14.649310788563));
#1800=CARTESIAN_POINT('Ctrl Pts',(3.301248674694,-24.027643879362,14.5347104556859));
#1801=CARTESIAN_POINT('Ctrl Pts',(2.7404244263817,-23.5183108657722,14.4774416377848));
#1802=CARTESIAN_POINT('Ctrl Pts',(1.44064112961331,-22.8212020237703,14.3628407459321));
#1803=CARTESIAN_POINT('Ctrl Pts',(0.702452411780137,-22.6354736977066,14.3055721519949));
#1804=CARTESIAN_POINT('Ctrl Pts',(-0.779472887126354,-22.6333352967227,
14.190970710093));
#1805=CARTESIAN_POINT('Ctrl Pts',(-1.52155253015143,-22.8183614641083,14.1337023369077));
#1806=CARTESIAN_POINT('Ctrl Pts',(-2.83570509877543,-23.5183020242021,14.0191003537129));
#1807=CARTESIAN_POINT('Ctrl Pts',(-3.40563177267265,-24.0336906113064,13.9618321981179));
#1808=CARTESIAN_POINT('Ctrl Pts',(-4.23859829449245,-25.2762621036854,13.8472296822221));
#1809=CARTESIAN_POINT('Ctrl Pts',(-4.49952012993745,-26.0028377560707,13.7899617411021));
#1810=CARTESIAN_POINT('Ctrl Pts',(-4.64912831734354,-27.4983091479623,13.6753587009413));
#1811=CARTESIAN_POINT('Ctrl Pts',(-4.53623796107103,-28.2656580682614,13.6180909712297));
#1812=CARTESIAN_POINT('Ctrl Pts',(-3.96059130788698,-29.6615610540449,13.5034874150766));
#1813=CARTESIAN_POINT('Ctrl Pts',(-3.49718400748527,-30.2879987021829,13.4462198937543));
#1814=CARTESIAN_POINT('Ctrl Pts',(-2.32610691316009,-31.2522011376172,13.3316158297333));
#1815=CARTESIAN_POINT('Ctrl Pts',(-1.61887397941475,-31.5877894623157,13.2743485138248));
#1816=CARTESIAN_POINT('Ctrl Pts',(-0.124698014175552,-31.8875168697119,
13.1597439499104));
#1817=CARTESIAN_POINT('Ctrl Pts',(0.660820605236803,-31.8499459440715,13.1024768364861));
#1818=CARTESIAN_POINT('Ctrl Pts',(2.12657161732859,-31.4079510480467,12.9878717805055));
#1819=CARTESIAN_POINT('Ctrl Pts',(2.8047317654823,-31.0026997016065,12.9306048666812));
#1820=CARTESIAN_POINT('Ctrl Pts',(3.89404127890867,-29.9170320609718,12.8159993263168));
#1821=CARTESIAN_POINT('Ctrl Pts',(4.30296864843086,-29.2368757228388,12.7587326092554));
#1822=CARTESIAN_POINT('Ctrl Pts',(4.75395585015817,-27.7592219594744,12.6441265920449));
#1823=CARTESIAN_POINT('Ctrl Pts',(4.79418068964257,-26.9630145561609,12.5868600689426));
#1824=CARTESIAN_POINT('Ctrl Pts',(4.49404010690874,-25.4403710926243,12.4722535823103));
#1825=CARTESIAN_POINT('Ctrl Pts',(4.15267254437464,-24.7159484861244,12.4149872504092));
#1826=CARTESIAN_POINT('Ctrl Pts',(3.16580254027823,-23.5091389781496,12.3003803016153));
#1827=CARTESIAN_POINT('Ctrl Pts',(2.52037754996715,-23.0290058774741,12.2431141582025));
#1828=CARTESIAN_POINT('Ctrl Pts',(1.07470328235808,-22.427176726376,12.1285067543989));
#1829=CARTESIAN_POINT('Ctrl Pts',(0.275598076802496,-22.3074311776151,12.0712407967975));
#1830=CARTESIAN_POINT('Ctrl Pts',(-1.84868379116737,-22.5127927449768,11.9157393755432));
#1831=CARTESIAN_POINT('Ctrl Pts',(-3.12606319175256,-23.2393767520925,11.8175853786087));
#1832=CARTESIAN_POINT('Ctrl Pts',(-4.33213271301493,-24.880386526967,11.6703268381421));
#1833=CARTESIAN_POINT('Ctrl Pts',(-4.61678084393395,-25.5145917668544,11.6212300753262));
#1834=CARTESIAN_POINT('Ctrl Pts',(-4.8325074990541,-26.51374965466,11.547605629606));
#1835=CARTESIAN_POINT('Ctrl Pts',(-4.86981537831802,-26.8545716453141,11.5230623381901));
#1836=CARTESIAN_POINT('Ctrl Pts',(-4.87150546249911,-27.5373956033118,11.4739637523339));
#1837=CARTESIAN_POINT('Ctrl Pts',(-4.84806449389349,-27.8775537395237,11.4494246411902));
#1838=CARTESIAN_POINT('Ctrl Pts',(-4.8332020483632,-28.2179636982637,11.4248805192881));
#1839=CARTESIAN_POINT('Ctrl Pts',(-4.49992531496781,-27.2005618150104,22.4987331790167));
#1840=CARTESIAN_POINT('Ctrl Pts',(-4.50123266577206,-27.9399345555106,22.4403537839278));
#1841=CARTESIAN_POINT('Ctrl Pts',(-4.31885456358521,-28.6714666153785,22.3845992765752));
#1842=CARTESIAN_POINT('Ctrl Pts',(-3.27206873853112,-30.6387455869407,22.2092430694354));
#1843=CARTESIAN_POINT('Ctrl Pts',(-1.90301347052226,-31.5589454854703,22.0978648836455));
#1844=CARTESIAN_POINT('Ctrl Pts',(1.08133745456905,-31.8588483286696,21.8641055935273));
#1845=CARTESIAN_POINT('Ctrl Pts',(2.62163729847883,-31.2259625043182,21.7526920522415));
#1846=CARTESIAN_POINT('Ctrl Pts',(4.54712383673962,-28.889667640373,21.5189807362004));
#1847=CARTESIAN_POINT('Ctrl Pts',(4.87991725612086,-27.2420071964223,21.4075326300492));
#1848=CARTESIAN_POINT('Ctrl Pts',(3.99926793651637,-24.3160463481836,21.1738683059317));
#1849=CARTESIAN_POINT('Ctrl Pts',(2.80324492166405,-23.1127118024641,21.0623863989465));
#1850=CARTESIAN_POINT('Ctrl Pts',(-0.145664295624094,-22.2108911563125,
20.8287681139101));
#1851=CARTESIAN_POINT('Ctrl Pts',(-1.82608753442347,-22.5396643242445,20.7172531447498));
#1852=CARTESIAN_POINT('Ctrl Pts',(-4.23617685498116,-24.5081432429562,20.4836799735107));
#1853=CARTESIAN_POINT('Ctrl Pts',(-4.90258935139331,-26.1024197715759,20.3721326565532));
#1854=CARTESIAN_POINT('Ctrl Pts',(-4.60239401978947,-29.2279523583354,20.1386037010885));
#1855=CARTESIAN_POINT('Ctrl Pts',(-3.63850146388098,-30.6809230335259,20.0270247275001));
#1856=CARTESIAN_POINT('Ctrl Pts',(-0.848312218451317,-32.1812843569572,
19.7935391153079));
#1857=CARTESIAN_POINT('Ctrl Pts',(0.910962191510308,-32.187257662144,19.6819291541039));
#1858=CARTESIAN_POINT('Ctrl Pts',(3.73351916376344,-30.6878849222468,19.4484860378945));
#1859=CARTESIAN_POINT('Ctrl Pts',(4.72474370347859,-29.2155039993741,19.3368457367663));
#1860=CARTESIAN_POINT('Ctrl Pts',(5.04923349895883,-26.0077171480983,19.103444293163));
#1861=CARTESIAN_POINT('Ctrl Pts',(4.36986673206198,-24.3509968931086,18.9917742794446));
#1862=CARTESIAN_POINT('Ctrl Pts',(1.86145168328288,-22.2810150440159,18.7584137083719));
#1863=CARTESIAN_POINT('Ctrl Pts',(0.0911844603756664,-21.9222328729832,
18.6467145899854));
#1864=CARTESIAN_POINT('Ctrl Pts',(-3.05047794174479,-22.8657614168808,18.4133941133931));
#1865=CARTESIAN_POINT('Ctrl Pts',(-4.3434939460169,-24.1492993667947,18.3016664794364));
#1866=CARTESIAN_POINT('Ctrl Pts',(-5.31279863706187,-27.3124610697944,18.0683853413922));
#1867=CARTESIAN_POINT('Ctrl Pts',(-4.96105242549078,-29.116041915327,17.9566297629436));
#1868=CARTESIAN_POINT('Ctrl Pts',(-2.85190795720616,-31.7012004702625,17.7233872278977));
#1869=CARTESIAN_POINT('Ctrl Pts',(-1.14247440761136,-32.4168925823255,17.6116042590234));
#1870=CARTESIAN_POINT('Ctrl Pts',(1.36942113919458,-32.1769364386145,17.4367007733733));
#1871=CARTESIAN_POINT('Ctrl Pts',(2.17863030294074,-31.8896680393015,17.3807991645495));
#1872=CARTESIAN_POINT('Ctrl Pts',(3.58594774059714,-30.955345510934,17.2642061815091));
#1873=CARTESIAN_POINT('Ctrl Pts',(4.1666380278044,-30.3178934995088,17.2082979257248));
#1874=CARTESIAN_POINT('Ctrl Pts',(4.97070480320723,-28.8243377732163,17.0917141975888));
#1875=CARTESIAN_POINT('Ctrl Pts',(5.18324736692089,-27.9849325707496,17.0357993595099));
#1876=CARTESIAN_POINT('Ctrl Pts',(5.18837634682399,-26.2816906794162,16.9192248016874));
#1877=CARTESIAN_POINT('Ctrl Pts',(4.97928961288882,-25.4377044137181,16.8633034450976));
#1878=CARTESIAN_POINT('Ctrl Pts',(4.17766130573194,-23.9269514586941,16.7467379739209));
#1879=CARTESIAN_POINT('Ctrl Pts',(3.59301796923098,-23.2784899136664,16.6908101616495));
#1880=CARTESIAN_POINT('Ctrl Pts',(2.16808835767185,-22.3200655571735,16.5742536948244));
#1881=CARTESIAN_POINT('Ctrl Pts',(1.34341569002319,-22.0225242875423,16.5183194887516));
#1882=CARTESIAN_POINT('Ctrl Pts',(-0.37202542262785,-21.848229520912,16.4017719448942));
#1883=CARTESIAN_POINT('Ctrl Pts',(-1.2431512747268,-21.9750627042462,16.3458314060321));
#1884=CARTESIAN_POINT('Ctrl Pts',(-2.84469319036191,-22.6326276198057,16.2292927049662));
#1885=CARTESIAN_POINT('Ctrl Pts',(-3.55608395141779,-23.1572481132965,16.1733458934499));
#1886=CARTESIAN_POINT('Ctrl Pts',(-4.66303405570225,-24.4975081087771,16.0568159559262));
#1887=CARTESIAN_POINT('Ctrl Pts',(-5.0446924336988,-25.2987711172549,16.0008629310603));
#1888=CARTESIAN_POINT('Ctrl Pts',(-5.39056519898843,-27.0094466251327,15.8843416789414));
#1889=CARTESIAN_POINT('Ctrl Pts',(-5.34930304043553,-27.8996098051487,15.8283824991195));
#1890=CARTESIAN_POINT('Ctrl Pts',(-4.84595092330871,-29.5780539034839,15.7118698553524));
#1891=CARTESIAN_POINT('Ctrl Pts',(-4.38811855967175,-30.3467642405488,15.6559045781531));
#1892=CARTESIAN_POINT('Ctrl Pts',(-3.14807661476919,-31.5947342749175,15.5394004666024));
#1893=CARTESIAN_POINT('Ctrl Pts',(-2.37886502949379,-32.0587365058605,15.4834291488454));
#1894=CARTESIAN_POINT('Ctrl Pts',(-0.690271412805203,-32.5768833169426,
15.3669334943444));
#1895=CARTESIAN_POINT('Ctrl Pts',(0.210437406783647,-32.6237032613599,15.3109561919855));
#1896=CARTESIAN_POINT('Ctrl Pts',(1.95077582228988,-32.2833593081943,15.1944689204932));
#1897=CARTESIAN_POINT('Ctrl Pts',(2.77047067840731,-31.8985499371097,15.1384856887274));
#1898=CARTESIAN_POINT('Ctrl Pts',(4.15032302098314,-30.7736043375475,15.0220067269618));
#1899=CARTESIAN_POINT('Ctrl Pts',(4.69400309684405,-30.0449584837519,14.9660176202321));
#1900=CARTESIAN_POINT('Ctrl Pts',(5.38335863834062,-28.395939593178,14.8495468960155));
#1901=CARTESIAN_POINT('Ctrl Pts',(5.51992097583071,-27.4934852178884,14.7935519679768));
#1902=CARTESIAN_POINT('Ctrl Pts',(5.34990401728289,-25.7072478702335,14.6770894099612));
#1903=CARTESIAN_POINT('Ctrl Pts',(5.04374456081733,-24.8435781449226,14.6210887135337));
#1904=CARTESIAN_POINT('Ctrl Pts',(4.0479320191368,-23.342552408645,14.5046342513644));
#1905=CARTESIAN_POINT('Ctrl Pts',(3.36814614645295,-22.7227447945842,14.4486278387742));
#1906=CARTESIAN_POINT('Ctrl Pts',(1.77619102970885,-21.8650344590564,14.3321814028423));
#1907=CARTESIAN_POINT('Ctrl Pts',(0.881013595157293,-21.6379564042767,14.2761693255965));
#1908=CARTESIAN_POINT('Ctrl Pts',(-0.934286602741275,-21.631913240891,14.1597308473328));
#1909=CARTESIAN_POINT('Ctrl Pts',(-1.83430603011931,-21.85447637771,14.1037131561842));
#1910=CARTESIAN_POINT('Ctrl Pts',(-3.44430347736566,-22.7081266226923,13.9872825678333));
#1911=CARTESIAN_POINT('Ctrl Pts',(-4.13582211102842,-23.3310704412515,13.9312593128857));
#1912=CARTESIAN_POINT('Ctrl Pts',(-5.15723598600513,-24.8486604334571,13.8148365475172));
#1913=CARTESIAN_POINT('Ctrl Pts',(-5.47468869489397,-25.7274061109226,13.7588077782201));
#1914=CARTESIAN_POINT('Ctrl Pts',(-5.66084498304722,-27.5542511137055,13.6423927697258));
#1915=CARTESIAN_POINT('Ctrl Pts',(-5.52607729259019,-28.4824463986154,13.5863585348362));
#1916=CARTESIAN_POINT('Ctrl Pts',(-4.82645265952584,-30.1878171234494,13.4699512180057));
#1917=CARTESIAN_POINT('Ctrl Pts',(-4.26793016275464,-30.9457917464557,13.4139115656321));
#1918=CARTESIAN_POINT('Ctrl Pts',(-2.84163338331343,-32.1244708835282,13.2975118759857));
#1919=CARTESIAN_POINT('Ctrl Pts',(-1.98851329456531,-32.5312245863753,13.2414668535995));
#1920=CARTESIAN_POINT('Ctrl Pts',(-0.168154346495923,-32.8997884885716,
13.1250747275302));
#1921=CARTESIAN_POINT('Ctrl Pts',(0.779568298212397,-32.8562079727566,13.0690243819638));
#1922=CARTESIAN_POINT('Ctrl Pts',(2.56542990953642,-32.3211571768756,12.9526397565944));
#1923=CARTESIAN_POINT('Ctrl Pts',(3.38380416962575,-31.8341443288812,12.8965841340846));
#1924=CARTESIAN_POINT('Ctrl Pts',(4.71155278837089,-30.5155103343138,12.7802069473221));
#1925=CARTESIAN_POINT('Ctrl Pts',(5.20559259369133,-29.6971531119313,12.7241460934996));
#1926=CARTESIAN_POINT('Ctrl Pts',(5.75703886090729,-27.9016459598323,12.6077762839981));
#1927=CARTESIAN_POINT('Ctrl Pts',(5.80717713818053,-26.9434385648419,12.5517102438793));
#1928=CARTESIAN_POINT('Ctrl Pts',(5.44579520263474,-25.0931237590171,12.4353477510898));
#1929=CARTESIAN_POINT('Ctrl Pts',(5.0368047411671,-24.2211610859936,12.3792765691091));
#1930=CARTESIAN_POINT('Ctrl Pts',(3.84146164273372,-22.7542474974693,12.2629213331626));
#1931=CARTESIAN_POINT('Ctrl Pts',(3.06685116348872,-22.1758765063834,12.2068450531984));
#1932=CARTESIAN_POINT('Ctrl Pts',(1.3147114679644,-21.4429359570459,12.0904970149672));
#1933=CARTESIAN_POINT('Ctrl Pts',(0.355369734306315,-21.2974519808943,12.0344156803179));
#1934=CARTESIAN_POINT('Ctrl Pts',(-2.21947927012219,-21.541945111076,11.8765628382364));
#1935=CARTESIAN_POINT('Ctrl Pts',(-3.75768230547338,-22.4163266113853,11.7792514363029));
#1936=CARTESIAN_POINT('Ctrl Pts',(-5.21498730250992,-24.3919766537203,11.6318625545005));
#1937=CARTESIAN_POINT('Ctrl Pts',(-5.56061254440886,-25.1583366949337,11.5821196744937));
#1938=CARTESIAN_POINT('Ctrl Pts',(-5.82237026188237,-26.3605430038448,11.5086720015383));
#1939=CARTESIAN_POINT('Ctrl Pts',(-5.86810470583882,-26.7709263784967,11.4841148639085));
#1940=CARTESIAN_POINT('Ctrl Pts',(-5.87151787372438,-27.5964966533761,11.4342490225503));
#1941=CARTESIAN_POINT('Ctrl Pts',(-5.8464491178956,-27.9182877595946,11.4098155239949));
#1942=CARTESIAN_POINT('Ctrl Pts',(-5.83158667236532,-28.2586977183358,11.3852714020937));
#1943=CARTESIAN_POINT('Ctrl Pts',(-4.49992531496781,-27.1010184425723,21.5036999549465));
#1944=CARTESIAN_POINT('Ctrl Pts',(-4.51674600628465,-27.8405511731054,21.4453045543583));
#1945=CARTESIAN_POINT('Ctrl Pts',(-4.3513754570227,-28.5765453512511,21.3895276624965));
#1946=CARTESIAN_POINT('Ctrl Pts',(-3.34502119885618,-30.5657740901924,21.2141080231263));
#1947=CARTESIAN_POINT('Ctrl Pts',(-1.99683196222126,-31.5170666924607,21.1026952188504));
#1948=CARTESIAN_POINT('Ctrl Pts',(0.980993279522333,-31.8772272555485,20.8688610765165));
#1949=CARTESIAN_POINT('Ctrl Pts',(2.53490239289457,-31.2787547245274,20.7574094693259));
#1950=CARTESIAN_POINT('Ctrl Pts',(4.50569444399399,-28.9816631968142,20.5236326621716));
#1951=CARTESIAN_POINT('Ctrl Pts',(4.87413701918684,-27.3422265898772,20.41214314674));
#1952=CARTESIAN_POINT('Ctrl Pts',(4.05086560996824,-24.4015014064168,20.1784223463925));
#1953=CARTESIAN_POINT('Ctrl Pts',(2.88154677707693,-23.173754043832,20.0668957873436));
#1954=CARTESIAN_POINT('Ctrl Pts',(-0.0470467715653138,-22.2169532717186,
19.8332297105388));
#1955=CARTESIAN_POINT('Ctrl Pts',(-1.73235777827075,-22.5102673549153,19.7216669438178));
#1956=CARTESIAN_POINT('Ctrl Pts',(-4.17572182242301,-24.4312269013205,19.4880543497385));
#1957=CARTESIAN_POINT('Ctrl Pts',(-4.87376845888169,-26.0095620732211,19.3764561838128));
#1958=CARTESIAN_POINT('Ctrl Pts',(-4.6310120681261,-29.1353686231182,19.1428958730047));
#1959=CARTESIAN_POINT('Ctrl Pts',(-3.69789395427398,-30.6051559498652,19.0312630900414));
#1960=CARTESIAN_POINT('Ctrl Pts',(-0.939901316815822,-32.1524297385279,
18.797753901872));
#1961=CARTESIAN_POINT('Ctrl Pts',(0.815770716897848,-32.192946710534,18.6860872589115));
#1962=CARTESIAN_POINT('Ctrl Pts',(3.65834639903831,-30.746287086809,18.4526280705631));
#1963=CARTESIAN_POINT('Ctrl Pts',(4.67570856491877,-29.2962834910467,18.3409283004432));
#1964=CARTESIAN_POINT('Ctrl Pts',(5.05445235298275,-26.1019770515496,18.1075180249339));
#1965=CARTESIAN_POINT('Ctrl Pts',(4.40805306181254,-24.4365392522985,17.9957858373769));
#1966=CARTESIAN_POINT('Ctrl Pts',(1.94130016670179,-22.3299662886282,17.7624234222861));
#1967=CARTESIAN_POINT('Ctrl Pts',(0.182492857305352,-21.939377617945,17.6506595049407));
#1968=CARTESIAN_POINT('Ctrl Pts',(-2.96543044577777,-22.8282401952741,17.4173439305767));
#1969=CARTESIAN_POINT('Ctrl Pts',(-4.27794385851622,-24.0844995025642,17.3055489496951));
#1970=CARTESIAN_POINT('Ctrl Pts',(-5.29537653242634,-27.2218242153782,17.0722792286103));
#1971=CARTESIAN_POINT('Ctrl Pts',(-4.97689278167529,-29.0259395054587,16.9604538299531));
#1972=CARTESIAN_POINT('Ctrl Pts',(-2.91608530249191,-31.6357336752382,16.7272290046934));
#1973=CARTESIAN_POINT('Ctrl Pts',(-1.22497985084763,-32.3788890909175,16.6153738146158));
#1974=CARTESIAN_POINT('Ctrl Pts',(1.28145612063066,-32.1789932923933,16.4404881713498));
#1975=CARTESIAN_POINT('Ctrl Pts',(2.0927818601203,-31.9069109397873,16.3845495671917));
#1976=CARTESIAN_POINT('Ctrl Pts',(3.50922640420288,-30.9978632225545,16.2679699605668));
#1977=CARTESIAN_POINT('Ctrl Pts',(4.09881550944335,-30.3728309488599,16.2120241353908));
#1978=CARTESIAN_POINT('Ctrl Pts',(4.92262783581331,-28.8973868790768,16.0954552401651));
#1979=CARTESIAN_POINT('Ctrl Pts',(5.14877399302525,-28.064821040575,16.0395022670422));
#1980=CARTESIAN_POINT('Ctrl Pts',(5.17972192673461,-26.3684552205223,15.9229439741396));
#1981=CARTESIAN_POINT('Ctrl Pts',(4.98580796318786,-25.5242055246215,15.8669839251149));
#1982=CARTESIAN_POINT('Ctrl Pts',(4.21017429044416,-24.0075929294983,15.7504361268929));
#1983=CARTESIAN_POINT('Ctrl Pts',(3.63880072013838,-23.351872300329,15.6944690729279));
#1984=CARTESIAN_POINT('Ctrl Pts',(2.23413550967172,-22.3762507712042,15.5779316635816));
#1985=CARTESIAN_POINT('Ctrl Pts',(1.41781408360257,-22.0661561590653,15.5219576745624));
#1986=CARTESIAN_POINT('Ctrl Pts',(-0.2876678119969,-21.8672909533799,15.4054305496812));
#1987=CARTESIAN_POINT('Ctrl Pts',(-1.15723576718454,-21.9791742088117,15.349449694498));
#1988=CARTESIAN_POINT('Ctrl Pts',(-2.76133682475571,-22.6104139372597,15.2329327513282));
#1989=CARTESIAN_POINT('Ctrl Pts',(-3.47827719059933,-23.1211141138698,15.1769450978676));
#1990=CARTESIAN_POINT('Ctrl Pts',(-4.59966549973914,-24.4392847330131,15.0604382350449));
#1991=CARTESIAN_POINT('Ctrl Pts',(-4.99267244674646,-25.2308278340738,15.0044438502435));
#1992=CARTESIAN_POINT('Ctrl Pts',(-5.36152867501004,-26.9286517721488,14.8879469679338));
#1993=CARTESIAN_POINT('Ctrl Pts',(-5.33479062947237,-27.815489816777,14.8319459176988));
#1994=CARTESIAN_POINT('Ctrl Pts',(-4.85770689425811,-29.4932029850683,14.7154589175941));
#1995=CARTESIAN_POINT('Ctrl Pts',(-4.41424130928336,-30.2657064039853,14.6594512668976));
#1996=CARTESIAN_POINT('Ctrl Pts',(-3.19776731478627,-31.5251842790945,14.5429740520141));
#1997=CARTESIAN_POINT('Ctrl Pts',(-2.43948640778453,-31.9991936236663,14.4869598649523));
#1998=CARTESIAN_POINT('Ctrl Pts',(-0.76641117646687,-32.538424291025,14.3704923396933));
#1999=CARTESIAN_POINT('Ctrl Pts',(0.129280639488567,-32.5991484080323,14.3144716793848));
#2000=CARTESIAN_POINT('Ctrl Pts',(1.86565117755554,-32.2846351962422,14.1980137496642));
#2001=CARTESIAN_POINT('Ctrl Pts',(2.6873584363981,-31.9144328140864,14.1419866783607));
#2002=CARTESIAN_POINT('Ctrl Pts',(4.0756575425974,-30.8141731242952,14.025538251239));
#2003=CARTESIAN_POINT('Ctrl Pts',(4.62788574697171,-30.0974982118229,13.9695048303297));
#2004=CARTESIAN_POINT('Ctrl Pts',(5.33614212196108,-28.4664074366612,13.8530658143517));
#2005=CARTESIAN_POINT('Ctrl Pts',(5.48580553915912,-27.5705664905401,13.7970261043234));
#2006=CARTESIAN_POINT('Ctrl Pts',(5.34081184824442,-25.791439376031,13.6805964092432));
#2007=CARTESIAN_POINT('Ctrl Pts',(5.04929361698828,-24.927539264489,13.6245504697451));
#2008=CARTESIAN_POINT('Ctrl Pts',(4.07891464172889,-23.4212168574546,13.5081300066553));
#2009=CARTESIAN_POINT('Ctrl Pts',(3.41195903484832,-22.794417393971,13.4520778965404));
#2010=CARTESIAN_POINT('Ctrl Pts',(1.84005664325852,-21.9202404356125,13.3356665776424));
#2011=CARTESIAN_POINT('Ctrl Pts',(0.952974962988242,-21.6810345955686,13.2796083549412));
#2012=CARTESIAN_POINT('Ctrl Pts',(-0.852207019879878,-21.6511301665541,
13.1632060938123));
#2013=CARTESIAN_POINT('Ctrl Pts',(-1.75069597922114,-21.8592211322789,13.1071418157038));
#2014=CARTESIAN_POINT('Ctrl Pts',(-3.36279321619093,-22.687065563139,12.9907485270725));
#2015=CARTESIAN_POINT('Ctrl Pts',(-4.0596712085529,-23.2965088909024,12.9346782499817));
#2016=CARTESIAN_POINT('Ctrl Pts',(-5.09490115062812,-24.7922309126811,12.8182938497412));
#2017=CARTESIAN_POINT('Ctrl Pts',(-5.42335290963779,-25.6615296657728,12.7622176293468));
#2018=CARTESIAN_POINT('Ctrl Pts',(-5.6318733184926,-27.4754205110425,12.6458420345123));
#2019=CARTESIAN_POINT('Ctrl Pts',(-5.51121048465282,-28.4003675711241,12.5897599257099));
#2020=CARTESIAN_POINT('Ctrl Pts',(-4.83738798718038,-30.1046366902265,12.4733930545196));
#2021=CARTESIAN_POINT('Ctrl Pts',(-4.29284127804266,-30.8662836546237,12.4173051114547));
#2022=CARTESIAN_POINT('Ctrl Pts',(-2.88989812922953,-32.0559489908963,12.3009468831881));
#2023=CARTESIAN_POINT('Ctrl Pts',(-2.04742969825749,-32.4724339533943,12.244853159285));
#2024=CARTESIAN_POINT('Ctrl Pts',(-0.2426536662203,-32.8615528897918,12.1285034943741));
#2025=CARTESIAN_POINT('Ctrl Pts',(0.700167228706349,-32.8315189484388,12.0724040423241));
#2026=CARTESIAN_POINT('Ctrl Pts',(2.48176316317964,-32.3218947112272,11.9560628622509));
#2027=CARTESIAN_POINT('Ctrl Pts',(3.30209026051788,-31.8491345603716,11.8999577340539));
#2028=CARTESIAN_POINT('Ctrl Pts',(4.63785467742761,-30.5549942620067,11.7836249613568));
#2029=CARTESIAN_POINT('Ctrl Pts',(5.14023670521377,-29.7483336343732,11.7275142083257));
#2030=CARTESIAN_POINT('Ctrl Pts',(5.71014369190083,-27.9707987230122,11.6111897665715));
#2031=CARTESIAN_POINT('Ctrl Pts',(5.77308874181379,-27.0190622633568,11.5550734393245));
#2032=CARTESIAN_POINT('Ctrl Pts',(5.43639437006847,-25.1760989492496,11.4387572531387));
#2033=CARTESIAN_POINT('Ctrl Pts',(5.04173404968112,-24.3039132848956,11.3826354016244));
#2034=CARTESIAN_POINT('Ctrl Pts',(3.87166745943498,-22.8320547671859,11.2663273965984));
#2035=CARTESIAN_POINT('Ctrl Pts',(3.10962740498996,-22.2468328201306,11.2102000701237));
#2036=CARTESIAN_POINT('Ctrl Pts',(1.3775808247441,-21.4977812085784,11.0939001728392));
#2037=CARTESIAN_POINT('Ctrl Pts',(0.426176004646674,-21.3404003073863,11.0377674200549));
#2038=CARTESIAN_POINT('Ctrl Pts',(-2.13467139062884,-21.5528754416251,10.8799811119317));
#2039=CARTESIAN_POINT('Ctrl Pts',(-3.67375330512296,-22.4019087871921,10.7826247286485));
#2040=CARTESIAN_POINT('Ctrl Pts',(-5.14572845587871,-24.3467779409998,10.6352234649416));
#2041=CARTESIAN_POINT('Ctrl Pts',(-5.4980087978572,-25.10396329861,10.585497622957));
#2042=CARTESIAN_POINT('Ctrl Pts',(-5.77284291612865,-26.2950238657267,10.5120341100286));
#2043=CARTESIAN_POINT('Ctrl Pts',(-5.82326382778836,-26.7021580375338,10.4874753114238));
#2044=CARTESIAN_POINT('Ctrl Pts',(-5.83613711196663,-27.5221379313639,10.4376301541696));
#2045=CARTESIAN_POINT('Ctrl Pts',(-5.80990657648216,-27.8448337026384,10.4131866340964));
#2046=CARTESIAN_POINT('Ctrl Pts',(-5.79504413095202,-28.1852436613808,10.3886425121934));
#2047=CARTESIAN_POINT('Ctrl Pts',(-3.5,-27.1131792176833,21.5024833879649));
#2048=CARTESIAN_POINT('Ctrl Pts',(-3.51479119919922,-27.6859453885664,21.4451837185487));
#2049=CARTESIAN_POINT('Ctrl Pts',(-3.3869826954375,-28.2639018202575,21.3878808596267));
#2050=CARTESIAN_POINT('Ctrl Pts',(-2.61104013965461,-29.8091522948055,21.2159741435134));
#2051=CARTESIAN_POINT('Ctrl Pts',(-1.55527081107218,-30.5598658867912,21.1013735009366));
#2052=CARTESIAN_POINT('Ctrl Pts',(0.7596584103706,-30.8465909355752,20.8721694081605));
#2053=CARTESIAN_POINT('Ctrl Pts',(1.98433800521209,-30.3798149635844,20.7575670418755));
#2054=CARTESIAN_POINT('Ctrl Pts',(3.52578602540974,-28.5931135200025,20.5283676296524));
#2055=CARTESIAN_POINT('Ctrl Pts',(3.8208190800791,-27.3005795704328,20.4137635916772));
#2056=CARTESIAN_POINT('Ctrl Pts',(3.18340034511317,-25.0004020130352,20.1845686868986));
#2057=CARTESIAN_POINT('Ctrl Pts',(2.26172892311522,-24.0264166801336,20.0699630275308));
#2058=CARTESIAN_POINT('Ctrl Pts',(-0.0310075805132356,-23.2709470686081,
19.840772464982));
#2059=CARTESIAN_POINT('Ctrl Pts',(-1.36774615552683,-23.4993356660845,19.7261652328664));
#2060=CARTESIAN_POINT('Ctrl Pts',(-3.29044999554861,-25.003443698954,19.4969788547815));
#2061=CARTESIAN_POINT('Ctrl Pts',(-3.84882652597964,-26.255889878113,19.3823700969656));
#2062=CARTESIAN_POINT('Ctrl Pts',(-3.66341653596594,-28.7171925636406,19.1531877526223));
#2063=CARTESIAN_POINT('Ctrl Pts',(-2.92366288113256,-29.8898022514147,19.0385775146034));
#2064=CARTESIAN_POINT('Ctrl Pts',(-0.750050065449063,-31.1155888685023,
18.8093990599493));
#2065=CARTESIAN_POINT('Ctrl Pts',(0.651110587682156,-31.1517796318851,18.6947873857344));
#2066=CARTESIAN_POINT('Ctrl Pts',(2.90172211077653,-30.0124147872479,18.4656126830036));
#2067=CARTESIAN_POINT('Ctrl Pts',(3.71853772096227,-28.8547645355866,18.3509996151738));
#2068=CARTESIAN_POINT('Ctrl Pts',(4.02392234264642,-26.3233804905586,18.1218285325501));
#2069=CARTESIAN_POINT('Ctrl Pts',(3.50918503257104,-24.9871031169595,18.0072141122992));
#2070=CARTESIAN_POINT('Ctrl Pts',(1.55288051607053,-23.3098136929698,17.7780465236243));
#2071=CARTESIAN_POINT('Ctrl Pts',(0.140896517323791,-22.9926200323223,17.6634307908027));
#2072=CARTESIAN_POINT('Ctrl Pts',(-2.36650964254058,-23.6955465860942,17.4342665752667));
#2073=CARTESIAN_POINT('Ctrl Pts',(-3.42532249325332,-24.7042160076948,17.319649568463));
#2074=CARTESIAN_POINT('Ctrl Pts',(-4.24151789226149,-27.205672166438,17.0904886102752));
#2075=CARTESIAN_POINT('Ctrl Pts',(-3.98794903777075,-28.6613021650618,16.9758703668355));
#2076=CARTESIAN_POINT('Ctrl Pts',(-2.34405122024042,-30.7505189403242,16.7467125550671));
#2077=CARTESIAN_POINT('Ctrl Pts',(-0.978754765971974,-31.3540484715026,
16.6320931111307));
#2078=CARTESIAN_POINT('Ctrl Pts',(1.02933886603348,-31.1972354808515,16.460227032321));
#2079=CARTESIAN_POINT('Ctrl Pts',(1.68709482472537,-30.9779968406706,16.4029168679907));
#2080=CARTESIAN_POINT('Ctrl Pts',(2.8240837151474,-30.2508925065775,16.2883402228593));
#2081=CARTESIAN_POINT('Ctrl Pts',(3.30314935266293,-29.7448544918448,16.2310297714992));
#2082=CARTESIAN_POINT('Ctrl Pts',(3.96627580118359,-28.5616040731508,16.116453854622));
#2083=CARTESIAN_POINT('Ctrl Pts',(4.15104388235541,-27.8860791480164,16.0591431204344));
#2084=CARTESIAN_POINT('Ctrl Pts',(4.17802239058402,-26.5231491652539,15.9445679195579));
#2085=CARTESIAN_POINT('Ctrl Pts',(4.02164463287101,-25.836899273559,15.8872569066736));
#2086=CARTESIAN_POINT('Ctrl Pts',(3.39969277305442,-24.6162176795914,15.7726824098211));
#2087=CARTESIAN_POINT('Ctrl Pts',(2.9359020278153,-24.0821430128742,15.7153711223063));
#2088=CARTESIAN_POINT('Ctrl Pts',(1.80627259289743,-23.295059368917,15.6007973177115));
#2089=CARTESIAN_POINT('Ctrl Pts',(1.14217129355625,-23.0415308728188,15.5434857595736));
#2090=CARTESIAN_POINT('Ctrl Pts',(-0.231877317222814,-22.8792861228552,
15.4289126357253));
#2091=CARTESIAN_POINT('Ctrl Pts',(-0.940537550161687,-22.9692999005262,
15.3716008109));
#2092=CARTESIAN_POINT('Ctrl Pts',(-2.23508230276584,-23.4765970744679,15.2570283565139));
#2093=CARTESIAN_POINT('Ctrl Pts',(-2.82042721228882,-23.8921601369938,15.1997162688729));
#2094=CARTESIAN_POINT('Ctrl Pts',(-3.72724254909164,-24.9550994865649,15.0851444728953));
#2095=CARTESIAN_POINT('Ctrl Pts',(-4.04904226418634,-25.6007082903028,15.0278321262568));
#2096=CARTESIAN_POINT('Ctrl Pts',(-4.34898179372202,-26.9722920315092,14.913260977831));
#2097=CARTESIAN_POINT('Ctrl Pts',(-4.32823823833014,-27.696864249156,14.8559483759565));
#2098=CARTESIAN_POINT('Ctrl Pts',(-3.94416673686108,-29.0543767984046,14.741377864454));
#2099=CARTESIAN_POINT('Ctrl Pts',(-3.58247834736109,-29.6866038630478,14.684065011041));
#2100=CARTESIAN_POINT('Ctrl Pts',(-2.59897553580158,-30.7075411869121,14.5694951260371));
#2101=CARTESIAN_POINT('Ctrl Pts',(-1.97893887953295,-31.0963900092535,14.5121820247212));
#2102=CARTESIAN_POINT('Ctrl Pts',(-0.62377058727827,-31.5350735702099,14.3976127560067));
#2103=CARTESIAN_POINT('Ctrl Pts',(0.109859887125028,-31.5858618602476,14.3402994103674));
#2104=CARTESIAN_POINT('Ctrl Pts',(1.51846868411767,-31.3325375520331,14.2257307479178));
#2105=CARTESIAN_POINT('Ctrl Pts',(2.19257064211805,-31.0299670824768,14.1684171614822));
#2106=CARTESIAN_POINT('Ctrl Pts',(3.32065975230898,-30.1381775844584,14.0538490954731));
#2107=CARTESIAN_POINT('Ctrl Pts',(3.77459621319051,-29.5507269915758,13.9965352717156));
#2108=CARTESIAN_POINT('Ctrl Pts',(4.35164549000208,-28.2261503388289,13.8819677925012));
#2109=CARTESIAN_POINT('Ctrl Pts',(4.47554085920862,-27.4906059318028,13.8246537348364));
#2110=CARTESIAN_POINT('Ctrl Pts',(4.35932633846837,-26.043646007592,13.7100868329779));
#2111=CARTESIAN_POINT('Ctrl Pts',(4.1206457473642,-25.3332578752253,13.6527725447744));
#2112=CARTESIAN_POINT('Ctrl Pts',(3.33223129728641,-24.106308328171,13.5382062109767));
#2113=CARTESIAN_POINT('Ctrl Pts',(2.78423731477771,-23.5899834651597,13.4808916955503));
#2114=CARTESIAN_POINT('Ctrl Pts',(1.50450674316234,-22.8764080003258,13.3663259207328));
#2115=CARTESIAN_POINT('Ctrl Pts',(0.774413779611081,-22.6785518889991,13.309011181339));
#2116=CARTESIAN_POINT('Ctrl Pts',(-0.69739330426496,-22.6525522223851,13.1944459565731));
#2117=CARTESIAN_POINT('Ctrl Pts',(-1.43794247925327,-22.8231062186778,13.1371309964266));
#2118=CARTESIAN_POINT('Ctrl Pts',(-2.7541948376007,-23.4972409646481,13.0225663129528));
#2119=CARTESIAN_POINT('Ctrl Pts',(-3.32948087019843,-23.9991290609593,12.9652511352145));
#2120=CARTESIAN_POINT('Ctrl Pts',(-4.17626345911414,-25.2198325829076,12.8506869844455));
#2121=CARTESIAN_POINT('Ctrl Pts',(-4.4481843446811,-25.936961310921,12.7933715922294));
#2122=CARTESIAN_POINT('Ctrl Pts',(-4.62015665278908,-27.4194785452993,12.6788079657272));
#2123=CARTESIAN_POINT('Ctrl Pts',(-4.52137115313415,-28.183579240772,12.621492362104));
#2124=CARTESIAN_POINT('Ctrl Pts',(-3.97152663554103,-29.5783806208201,12.5069292515898));
#2125=CARTESIAN_POINT('Ctrl Pts',(-3.5220951227733,-30.2084906103522,12.4496134395774));
#2126=CARTESIAN_POINT('Ctrl Pts',(-2.37437165907619,-31.183679244984,12.3350508369351));
#2127=CARTESIAN_POINT('Ctrl Pts',(-1.67779038310627,-31.5289988293348,12.277734819509));
#2128=CARTESIAN_POINT('Ctrl Pts',(-0.199197333900588,-31.8492812709321,
12.1631727167557));
#2129=CARTESIAN_POINT('Ctrl Pts',(0.581419535730091,-31.825256919753,12.1058564968451));
#2130=CARTESIAN_POINT('Ctrl Pts',(2.04290487097247,-31.4086885823989,11.9912948861633));
#2131=CARTESIAN_POINT('Ctrl Pts',(2.72301785637377,-31.017689933097,11.9339784666505));
#2132=CARTESIAN_POINT('Ctrl Pts',(3.82034316796606,-29.9565159886648,11.8194173403514));
#2133=CARTESIAN_POINT('Ctrl Pts',(4.23761275995296,-29.2880562452814,11.7621007240815));
#2134=CARTESIAN_POINT('Ctrl Pts',(4.70706068115205,-27.8283747226536,11.6475400746183));
#2135=CARTESIAN_POINT('Ctrl Pts',(4.76009229327592,-27.0386382546772,11.5902232643864));
#2136=CARTESIAN_POINT('Ctrl Pts',(4.48463927434238,-25.5233462828554,11.4756630843606));
#2137=CARTESIAN_POINT('Ctrl Pts',(4.15760185288866,-24.7987006850272,11.4183460829245));
#2138=CARTESIAN_POINT('Ctrl Pts',(3.19600835697949,-23.5869462478655,11.3037863650511));
#2139=CARTESIAN_POINT('Ctrl Pts',(2.56315379146772,-23.099962191222,11.2464691751292));
#2140=CARTESIAN_POINT('Ctrl Pts',(1.13757263913847,-22.4820219779078,11.1319099122695));
#2141=CARTESIAN_POINT('Ctrl Pts',(0.346404347142174,-22.3503795041057,11.0745925365344));
#2142=CARTESIAN_POINT('Ctrl Pts',(-1.76387591167285,-22.5237230755283,10.9191576492385));
#2143=CARTESIAN_POINT('Ctrl Pts',(-3.04213419140331,-23.2249589278969,10.8209586709532));
#2144=CARTESIAN_POINT('Ctrl Pts',(-4.26287386638314,-24.8351878142477,10.6736877485838));
#2145=CARTESIAN_POINT('Ctrl Pts',(-4.55417709738229,-25.4602183705301,10.6246080237907));
#2146=CARTESIAN_POINT('Ctrl Pts',(-4.78298015330037,-26.4482305165422,10.5509677380958));
#2147=CARTESIAN_POINT('Ctrl Pts',(-4.82497450026767,-26.7858033043513,10.5264227857054));
#2148=CARTESIAN_POINT('Ctrl Pts',(-4.83612470074125,-27.4630368812996,10.4773448839533));
#2149=CARTESIAN_POINT('Ctrl Pts',(-4.81152195248019,-27.8040996825675,10.4527957512917));
#2150=CARTESIAN_POINT('Ctrl Pts',(-4.7966595069499,-28.1445096413087,10.4282516293878));
#2151=CARTESIAN_POINT('',(-3.5,-27.1131792176833,21.5024833879649));
#2152=CARTESIAN_POINT('',(-3.5,-27.2127225901214,22.4975166120351));
#2153=CARTESIAN_POINT('Origin',(-3.5,-27.1629509039024,22.));
#2154=CARTESIAN_POINT('',(-4.8706353805564,-27.2129260271478,11.4970938327966));
#2155=CARTESIAN_POINT('Ctrl Pts',(-3.5,-27.2127225901214,22.4975166120351));
#2156=CARTESIAN_POINT('Ctrl Pts',(-3.49927785868713,-27.7853287709716,22.4402329481162));
#2157=CARTESIAN_POINT('Ctrl Pts',(-3.35446180200001,-28.3588230843844,22.3829524737063));
#2158=CARTESIAN_POINT('Ctrl Pts',(-3.08233709444319,-28.8665899867746,22.3256713790777));
#2159=CARTESIAN_POINT('Ctrl Pts',(-2.53808767932955,-29.8821237915549,22.2111091898206));
#2160=CARTESIAN_POINT('Ctrl Pts',(-1.46145231937318,-30.6017446798008,22.0965431657326));
#2161=CARTESIAN_POINT('Ctrl Pts',(-0.300724866977927,-30.7149783442486,
21.9819785454515));
#2162=CARTESIAN_POINT('Ctrl Pts',(0.860002585417323,-30.8282120086964,21.8674139251703));
#2163=CARTESIAN_POINT('Ctrl Pts',(2.07107291079633,-30.3270227433741,21.752849624791));
#2164=CARTESIAN_POINT('Ctrl Pts',(2.81914416447585,-29.4140703534682,21.6382826642361));
#2165=CARTESIAN_POINT('Ctrl Pts',(3.56721541815537,-28.5011179635623,21.5237157036811));
#2166=CARTESIAN_POINT('Ctrl Pts',(3.82659931701312,-27.20036017698,21.4091530749885));
#2167=CARTESIAN_POINT('Ctrl Pts',(3.47920099433721,-26.05765356589,21.2945838607121));
#2168=CARTESIAN_POINT('Ctrl Pts',(3.13180267166131,-24.9149469548,21.1800146464357));
#2169=CARTESIAN_POINT('Ctrl Pts',(2.18342706770339,-23.9653744387647,21.0654536391327));
#2170=CARTESIAN_POINT('Ctrl Pts',(1.02690098156517,-23.6151296959839,20.9508822537436));
#2171=CARTESIAN_POINT('Ctrl Pts',(-0.129625104573071,-23.2648849532031,
20.8363108683544));
#2172=CARTESIAN_POINT('Ctrl Pts',(-1.46147591168062,-23.5287326354126,20.7217514337973));
#2173=CARTESIAN_POINT('Ctrl Pts',(-2.40619046989316,-24.3045463380016,20.6071779561761));
#2174=CARTESIAN_POINT('Ctrl Pts',(-3.35090502810569,-25.0803600405907,20.4926044785548));
#2175=CARTESIAN_POINT('Ctrl Pts',(-3.87764741849126,-26.3487475764667,20.3780465697071));
#2176=CARTESIAN_POINT('Ctrl Pts',(-3.75622295306029,-27.5792619376628,20.2634710752061));
#2177=CARTESIAN_POINT('Ctrl Pts',(-3.63479848762931,-28.8097762988588,20.148895580705));
#2178=CARTESIAN_POINT('Ctrl Pts',(-2.86427039073957,-29.9655693350743,20.0343391520621));
#2179=CARTESIAN_POINT('Ctrl Pts',(-1.76136567891206,-30.5550064110035,19.9197617127236));
#2180=CARTESIAN_POINT('Ctrl Pts',(-0.658460967084561,-31.1444434869326,
19.8051842733852));
#2181=CARTESIAN_POINT('Ctrl Pts',(0.746302062294618,-31.1460905834951,19.6906292809279));
#2182=CARTESIAN_POINT('Ctrl Pts',(1.86159846889728,-30.5500516030908,19.5760499656309));
#2183=CARTESIAN_POINT('Ctrl Pts',(2.97689487550167,-29.9540126226856,19.4614706503338));
#2184=CARTESIAN_POINT('Ctrl Pts',(3.76757285952208,-28.7739850439139,19.3469170514958));
#2185=CARTESIAN_POINT('Ctrl Pts',(3.89313817407229,-27.5015528155106,19.232335926138));
#2186=CARTESIAN_POINT('Ctrl Pts',(4.0187034886225,-26.2291205871072,19.1177548007802));
#2187=CARTESIAN_POINT('Ctrl Pts',(3.47099870281935,-24.9015607577697,19.0032025543658));
#2188=CARTESIAN_POINT('Ctrl Pts',(2.47201536773451,-24.0812116030623,18.8886196820384));
#2189=CARTESIAN_POINT('Ctrl Pts',(1.47303203265275,-23.2608624483575,18.7740368097113));
#2190=CARTESIAN_POINT('Ctrl Pts',(0.0495881203952367,-22.9754752873616,
18.6594858758451));
#2191=CARTESIAN_POINT('Ctrl Pts',(-1.20098450905675,-23.3542715475307,18.5449013169653));
#2192=CARTESIAN_POINT('Ctrl Pts',(-2.45155713850874,-23.7330678076998,18.4303167580854));
#2193=CARTESIAN_POINT('Ctrl Pts',(-3.49087258075458,-24.7690158719264,18.3157670982032));
#2194=CARTESIAN_POINT('Ctrl Pts',(-3.87490628882521,-26.0326624463887,18.2011809106308));
#2195=CARTESIAN_POINT('Ctrl Pts',(-4.25893999689644,-27.296309020853,18.0865947230583));
#2196=CARTESIAN_POINT('Ctrl Pts',(-3.97210868158914,-28.7514045749302,17.9720462998272));
#2197=CARTESIAN_POINT('Ctrl Pts',(-3.12599127827046,-29.7836951551393,17.8574585390487));
#2198=CARTESIAN_POINT('Ctrl Pts',(-2.27987387495177,-30.8159857353485,17.7428707782702));
#2199=CARTESIAN_POINT('Ctrl Pts',(-0.896249322735716,-31.3920519629118,
17.6283235555406));
#2200=CARTESIAN_POINT('Ctrl Pts',(0.446119482153031,-31.260803072352,17.5137342747424));
#2201=CARTESIAN_POINT('Ctrl Pts',(1.11730388459739,-31.1951786270721,17.4564396343434));
#2202=CARTESIAN_POINT('Ctrl Pts',(1.77294326754582,-30.9607539401843,17.3991664653485));
#2203=CARTESIAN_POINT('Ctrl Pts',(2.33687415954374,-30.584564367571,17.341871454575));
#2204=CARTESIAN_POINT('Ctrl Pts',(2.90080505154166,-30.2083747949576,17.2845764438015));
#2205=CARTESIAN_POINT('Ctrl Pts',(3.37097187102429,-29.6899170424932,17.2273035618313));
#2206=CARTESIAN_POINT('Ctrl Pts',(3.69266231980076,-29.0892360048921,17.1700081869394));
#2207=CARTESIAN_POINT('Ctrl Pts',(4.01435276857722,-28.4885549672909,17.1127128120475));
#2208=CARTESIAN_POINT('Ctrl Pts',(4.1855172562512,-27.8061906781911,17.0554402129015));
#2209=CARTESIAN_POINT('Ctrl Pts',(4.18609703346223,-27.1212876511694,16.9981444800039));
#2210=CARTESIAN_POINT('Ctrl Pts',(4.18667681067326,-26.4363846241478,16.9408487471063));
#2211=CARTESIAN_POINT('Ctrl Pts',(4.01512628257138,-25.7503981626563,16.8835764266556));
#2212=CARTESIAN_POINT('Ctrl Pts',(3.69115303545709,-25.1429871857214,16.8262803417527));
#2213=CARTESIAN_POINT('Ctrl Pts',(3.36717978834281,-24.5355762087865,16.7689842568497));
#2214=CARTESIAN_POINT('Ctrl Pts',(2.8901192769073,-24.0087606262116,16.7117122110268));
#2215=CARTESIAN_POINT('Ctrl Pts',(2.31517235890273,-23.6238173905489,16.6544157799911));
#2216=CARTESIAN_POINT('Ctrl Pts',(1.74022544089816,-23.2388741548863,16.5971193489555));
#2217=CARTESIAN_POINT('Ctrl Pts',(1.06777289997686,-22.997899001297,16.5398475737628));
#2218=CARTESIAN_POINT('Ctrl Pts',(0.375768986061547,-22.9290618458416,16.4825508023506));
#2219=CARTESIAN_POINT('Ctrl Pts',(-0.316234927853762,-22.8602246903861,
16.4252540309383));
#2220=CARTESIAN_POINT('Ctrl Pts',(-1.02645305770396,-22.9651883959601,16.3679825224341));
#2221=CARTESIAN_POINT('Ctrl Pts',(-1.67244586303799,-23.2319995764873,16.310685416293));
#2222=CARTESIAN_POINT('Ctrl Pts',(-2.31843866837203,-23.4988107570144,16.253388310152));
#2223=CARTESIAN_POINT('Ctrl Pts',(-2.89823397310667,-23.9282941364198,16.196117064454));
#2224=CARTESIAN_POINT('Ctrl Pts',(-3.34442253908102,-24.4708084993747,16.1388196291159));
#2225=CARTESIAN_POINT('Ctrl Pts',(-3.79061110505536,-25.0133228623296,16.0815221937778));
#2226=CARTESIAN_POINT('Ctrl Pts',(-4.10106225113868,-25.6686515734845,16.0242512070742));
#2227=CARTESIAN_POINT('Ctrl Pts',(-4.23954028441954,-26.3608692289885,15.9669534479561));
#2228=CARTESIAN_POINT('Ctrl Pts',(-4.37801831770041,-27.0530868844925,15.909655688838));
#2229=CARTESIAN_POINT('Ctrl Pts',(-4.34275064929299,-27.7809842375283,15.8523849573772));
#2230=CARTESIAN_POINT('Ctrl Pts',(-4.13758070760249,-28.4601059771739,15.7950868797947));
#2231=CARTESIAN_POINT('Ctrl Pts',(-3.93241076591198,-29.1392277168195,15.7377888022123));
#2232=CARTESIAN_POINT('Ctrl Pts',(-3.55635559774948,-29.7676616996119,15.6805183222975));
#2233=CARTESIAN_POINT('Ctrl Pts',(-3.05282021676699,-30.2723764411732,15.623219931461));
#2234=CARTESIAN_POINT('Ctrl Pts',(-2.5492848357845,-30.7770911827345,15.5659215406245));
#2235=CARTESIAN_POINT('Ctrl Pts',(-1.91831750124282,-31.1559328914483,15.508651308613));
#2236=CARTESIAN_POINT('Ctrl Pts',(-1.2329741624294,-31.3647327437876,15.451352609636));
#2237=CARTESIAN_POINT('Ctrl Pts',(-0.547630823615978,-31.5735325961269,
15.3940539106591));
#2238=CARTESIAN_POINT('Ctrl Pts',(0.191016654419482,-31.6104167135758,15.3367839229662));
#2239=CARTESIAN_POINT('Ctrl Pts',(0.89730499163605,-31.4708391887802,15.2794849208574));
#2240=CARTESIAN_POINT('Ctrl Pts',(1.60359332885263,-31.3312616639846,15.2221859187487));
#2241=CARTESIAN_POINT('Ctrl Pts',(2.27568288412789,-31.0140842055001,15.1649161718489));
#2242=CARTESIAN_POINT('Ctrl Pts',(2.83550405741099,-30.5558465016054,15.1076168715224));
#2243=CARTESIAN_POINT('Ctrl Pts',(3.39532523069409,-30.0976087977106,15.0503175711959));
#2244=CARTESIAN_POINT('Ctrl Pts',(3.84071356306252,-29.4981872635055,14.9930480616187));
#2245=CARTESIAN_POINT('Ctrl Pts',(4.11978778472223,-28.8269348794253,14.9357484678916));
#2246=CARTESIAN_POINT('Ctrl Pts',(4.39886200638193,-28.1556824953451,14.8784488741644));
#2247=CARTESIAN_POINT('Ctrl Pts',(4.50965629588013,-27.4135246591517,14.821179598491));
#2248=CARTESIAN_POINT('Ctrl Pts',(4.43903740169352,-26.6864895804728,14.7638797160928));
#2249=CARTESIAN_POINT('Ctrl Pts',(4.36841850750692,-25.9594545017938,14.7065798336947));
#2250=CARTESIAN_POINT('Ctrl Pts',(4.11509669119356,-25.2492967556584,14.649310788563));
#2251=CARTESIAN_POINT('Ctrl Pts',(3.70817268294378,-24.6384703175102,14.5920106221244));
#2252=CARTESIAN_POINT('Ctrl Pts',(3.301248674694,-24.027643879362,14.5347104556859));
#2253=CARTESIAN_POINT('Ctrl Pts',(2.7404244263817,-23.5183108657722,14.4774416377848));
#2254=CARTESIAN_POINT('Ctrl Pts',(2.09053277799751,-23.1697564447712,14.4201411918584));
#2255=CARTESIAN_POINT('Ctrl Pts',(1.44064112961332,-22.8212020237703,14.3628407459321));
#2256=CARTESIAN_POINT('Ctrl Pts',(0.702452411780131,-22.6354736977066,14.3055721519949));
#2257=CARTESIAN_POINT('Ctrl Pts',(-0.0385102376731089,-22.6344044972146,
14.2482714310439));
#2258=CARTESIAN_POINT('Ctrl Pts',(-0.779472887126349,-22.6333352967227,
14.190970710093));
#2259=CARTESIAN_POINT('Ctrl Pts',(-1.52155253015144,-22.8183614641083,14.1337023369077));
#2260=CARTESIAN_POINT('Ctrl Pts',(-2.17862881446343,-23.1683317441552,14.0764013453103));
#2261=CARTESIAN_POINT('Ctrl Pts',(-2.83570509877542,-23.5183020242021,14.0191003537129));
#2262=CARTESIAN_POINT('Ctrl Pts',(-3.40563177267264,-24.0336906113065,13.9618321981179));
#2263=CARTESIAN_POINT('Ctrl Pts',(-3.82211503358254,-24.6549763574959,13.90453094017));
#2264=CARTESIAN_POINT('Ctrl Pts',(-4.23859829449244,-25.2762621036854,13.8472296822221));
#2265=CARTESIAN_POINT('Ctrl Pts',(-4.49952012993745,-26.0028377560707,13.7899617411021));
#2266=CARTESIAN_POINT('Ctrl Pts',(-4.5743242236405,-26.7505734520165,13.7326602210217));
#2267=CARTESIAN_POINT('Ctrl Pts',(-4.64912831734354,-27.4983091479623,13.6753587009413));
#2268=CARTESIAN_POINT('Ctrl Pts',(-4.53623796107103,-28.2656580682613,13.6180909712297));
#2269=CARTESIAN_POINT('Ctrl Pts',(-4.248414634479,-28.9636095611531,13.5607891931531));
#2270=CARTESIAN_POINT('Ctrl Pts',(-3.96059130788698,-29.6615610540449,13.5034874150766));
#2271=CARTESIAN_POINT('Ctrl Pts',(-3.49718400748527,-30.2879987021829,13.4462198937543));
#2272=CARTESIAN_POINT('Ctrl Pts',(-2.91164546032268,-30.7700999199001,13.3889178617438));
#2273=CARTESIAN_POINT('Ctrl Pts',(-2.32610691316009,-31.2522011376172,13.3316158297333));
#2274=CARTESIAN_POINT('Ctrl Pts',(-1.61887397941474,-31.5877894623157,13.2743485138248));
#2275=CARTESIAN_POINT('Ctrl Pts',(-0.87178599679515,-31.7376531660138,13.2170462318676));
#2276=CARTESIAN_POINT('Ctrl Pts',(-0.124698014175558,-31.8875168697119,
13.1597439499104));
#2277=CARTESIAN_POINT('Ctrl Pts',(0.660820605236809,-31.8499459440715,13.1024768364861));
#2278=CARTESIAN_POINT('Ctrl Pts',(1.3936961112827,-31.6289484960591,13.0451743084958));
#2279=CARTESIAN_POINT('Ctrl Pts',(2.12657161732859,-31.4079510480467,12.9878717805055));
#2280=CARTESIAN_POINT('Ctrl Pts',(2.8047317654823,-31.0026997016065,12.9306048666813));
#2281=CARTESIAN_POINT('Ctrl Pts',(3.34938652219548,-30.4598658812891,12.873302096499));
#2282=CARTESIAN_POINT('Ctrl Pts',(3.89404127890866,-29.9170320609718,12.8159993263168));
#2283=CARTESIAN_POINT('Ctrl Pts',(4.30296864843085,-29.2368757228388,12.7587326092554));
#2284=CARTESIAN_POINT('Ctrl Pts',(4.5284622492945,-28.4980488411566,12.7014296006501));
#2285=CARTESIAN_POINT('Ctrl Pts',(4.75395585015816,-27.7592219594744,12.6441265920449));
#2286=CARTESIAN_POINT('Ctrl Pts',(4.79418068964257,-26.9630145561609,12.5868600689426));
#2287=CARTESIAN_POINT('Ctrl Pts',(4.64411039827566,-26.2016928243926,12.5295568256265));
#2288=CARTESIAN_POINT('Ctrl Pts',(4.49404010690874,-25.4403710926243,12.4722535823103));
#2289=CARTESIAN_POINT('Ctrl Pts',(4.15267254437464,-24.7159484861244,12.4149872504092));
#2290=CARTESIAN_POINT('Ctrl Pts',(3.65923754232643,-24.112543732137,12.3576837760122));
#2291=CARTESIAN_POINT('Ctrl Pts',(3.16580254027822,-23.5091389781496,12.3003803016153));
#2292=CARTESIAN_POINT('Ctrl Pts',(2.52037754996714,-23.0290058774741,12.2431141582024));
#2293=CARTESIAN_POINT('Ctrl Pts',(1.79754041616261,-22.7280913019251,12.1858104563006));
#2294=CARTESIAN_POINT('Ctrl Pts',(1.07470328235808,-22.427176726376,12.1285067543989));
#2295=CARTESIAN_POINT('Ctrl Pts',(0.275598076802497,-22.3074311776151,12.0712407967975));
#2296=CARTESIAN_POINT('Ctrl Pts',(-0.507222361580798,-22.3831090971102,
12.0139368708962));
#2297=CARTESIAN_POINT('Ctrl Pts',(-1.84868379116738,-22.5127927449768,11.9157393755432));
#2298=CARTESIAN_POINT('Ctrl Pts',(-3.12606319175256,-23.2393767520925,11.8175853786087));
#2299=CARTESIAN_POINT('Ctrl Pts',(-3.93010953926081,-24.3333832686755,11.7194130182977));
#2300=CARTESIAN_POINT('Ctrl Pts',(-4.33213271301493,-24.8803865269671,11.6703268381421));
#2301=CARTESIAN_POINT('Ctrl Pts',(-4.61678084393395,-25.5145917668544,11.6212300753262));
#2302=CARTESIAN_POINT('Ctrl Pts',(-4.76059861401404,-26.1806970253915,11.5721471115128));
#2303=CARTESIAN_POINT('Ctrl Pts',(-4.8325074990541,-26.51374965466,11.5476056296061));
#2304=CARTESIAN_POINT('Ctrl Pts',(-4.86981537831802,-26.8545716453141,11.5230623381901));
#2305=CARTESIAN_POINT('Ctrl Pts',(-4.87066042040856,-27.195983624313,11.498513045262));
#2306=CARTESIAN_POINT('Ctrl Pts',(-4.8706744167737,-27.2016384038463,11.4981064372701));
#2307=CARTESIAN_POINT('Ctrl Pts',(-4.87068176644947,-27.207292836302,11.4976998360475));
#2308=CARTESIAN_POINT('Ctrl Pts',(-4.87064344737806,-27.2129433732647,11.4972950499307));
#2309=CARTESIAN_POINT('',(-4.85063011250931,-27.2127229045708,11.4975165893541));
#2310=CARTESIAN_POINT('Origin',(-4.85063016993195,-27.162950903902,11.));
#2311=CARTESIAN_POINT('',(-4.83035516948488,-27.1129735823552,10.5029173190626));
#2312=CARTESIAN_POINT('Origin',(-4.85063016993195,-27.162950903902,11.));
#2313=CARTESIAN_POINT('Ctrl Pts',(-3.5,-27.1131792176833,21.5024833879649));
#2314=CARTESIAN_POINT('Ctrl Pts',(-3.51479119919922,-27.6859453885664,21.4451837185487));
#2315=CARTESIAN_POINT('Ctrl Pts',(-3.3869826954375,-28.2639018202575,21.3878808596267));
#2316=CARTESIAN_POINT('Ctrl Pts',(-3.1283351768432,-28.7789853117735,21.3305786209223));
#2317=CARTESIAN_POINT('Ctrl Pts',(-2.6110401396546,-29.8091522948055,21.2159741435134));
#2318=CARTESIAN_POINT('Ctrl Pts',(-1.55527081107218,-30.5598658867912,21.1013735009366));
#2319=CARTESIAN_POINT('Ctrl Pts',(-0.397806200350788,-30.7032284111832,
20.9867714545485));
#2320=CARTESIAN_POINT('Ctrl Pts',(0.7596584103706,-30.8465909355753,20.8721694081605));
#2321=CARTESIAN_POINT('Ctrl Pts',(1.98433800521209,-30.3798149635844,20.7575670418755));
#2322=CARTESIAN_POINT('Ctrl Pts',(2.75506201531091,-29.4864642417935,20.6429673357639));
#2323=CARTESIAN_POINT('Ctrl Pts',(3.52578602540974,-28.5931135200026,20.5283676296524));
#2324=CARTESIAN_POINT('Ctrl Pts',(3.8208190800791,-27.3005795704328,20.4137635916772));
#2325=CARTESIAN_POINT('Ctrl Pts',(3.50210971259614,-26.150490791734,20.2991661392879));
#2326=CARTESIAN_POINT('Ctrl Pts',(3.18340034511317,-25.0004020130352,20.1845686868986));
#2327=CARTESIAN_POINT('Ctrl Pts',(2.26172892311522,-24.0264166801336,20.0699630275308));
#2328=CARTESIAN_POINT('Ctrl Pts',(1.115360671301,-23.6486818743709,19.9553677462564));
#2329=CARTESIAN_POINT('Ctrl Pts',(-0.0310075805132359,-23.2709470686081,
19.840772464982));
#2330=CARTESIAN_POINT('Ctrl Pts',(-1.36774615552683,-23.4993356660845,19.7261652328664));
#2331=CARTESIAN_POINT('Ctrl Pts',(-2.32909807553772,-24.2513896825192,19.6115720438239));
#2332=CARTESIAN_POINT('Ctrl Pts',(-3.29044999554861,-25.003443698954,19.4969788547815));
#2333=CARTESIAN_POINT('Ctrl Pts',(-3.84882652597964,-26.255889878113,19.3823700969656));
#2334=CARTESIAN_POINT('Ctrl Pts',(-3.75612153097279,-27.4865412208768,19.267778924794));
#2335=CARTESIAN_POINT('Ctrl Pts',(-3.66341653596594,-28.7171925636406,19.1531877526223));
#2336=CARTESIAN_POINT('Ctrl Pts',(-2.92366288113256,-29.8898022514147,19.0385775146034));
#2337=CARTESIAN_POINT('Ctrl Pts',(-1.83685647329081,-30.5026955599585,18.9239882872764));
#2338=CARTESIAN_POINT('Ctrl Pts',(-0.750050065449064,-31.1155888685022,
18.8093990599493));
#2339=CARTESIAN_POINT('Ctrl Pts',(0.651110587682155,-31.1517796318851,18.6947873857344));
#2340=CARTESIAN_POINT('Ctrl Pts',(1.77641634922847,-30.5820972095669,18.5802000343691));
#2341=CARTESIAN_POINT('Ctrl Pts',(2.90172211077653,-30.0124147872479,18.4656126830036));
#2342=CARTESIAN_POINT('Ctrl Pts',(3.71853772096226,-28.8547645355866,18.3509996151738));
#2343=CARTESIAN_POINT('Ctrl Pts',(3.87123003180434,-27.5890725130726,18.236414073862));
#2344=CARTESIAN_POINT('Ctrl Pts',(4.02392234264641,-26.3233804905586,18.1218285325501));
#2345=CARTESIAN_POINT('Ctrl Pts',(3.50918503257104,-24.9871031169595,18.0072141122992));
#2346=CARTESIAN_POINT('Ctrl Pts',(2.53103277431928,-24.1484584049633,17.8926303179616));
#2347=CARTESIAN_POINT('Ctrl Pts',(1.55288051607053,-23.3098136929698,17.7780465236243));
#2348=CARTESIAN_POINT('Ctrl Pts',(0.140896517323788,-22.9926200323223,17.6634307908027));
#2349=CARTESIAN_POINT('Ctrl Pts',(-1.1128065626084,-23.3440833092083,17.5488486830347));
#2350=CARTESIAN_POINT('Ctrl Pts',(-2.36650964254058,-23.6955465860942,17.4342665752667));
#2351=CARTESIAN_POINT('Ctrl Pts',(-3.42532249325332,-24.7042160076948,17.319649568463));
#2352=CARTESIAN_POINT('Ctrl Pts',(-3.83342019275709,-25.9549440870654,17.2050690893692));
#2353=CARTESIAN_POINT('Ctrl Pts',(-4.24151789226148,-27.205672166438,17.0904886102752));
#2354=CARTESIAN_POINT('Ctrl Pts',(-3.98794903777076,-28.6613021650618,16.9758703668355));
#2355=CARTESIAN_POINT('Ctrl Pts',(-3.16600012900559,-29.705910552693,16.8612914609513));
#2356=CARTESIAN_POINT('Ctrl Pts',(-2.34405122024042,-30.7505189403242,16.7467125550671));
#2357=CARTESIAN_POINT('Ctrl Pts',(-0.978754765971974,-31.3540484715026,
16.6320931111307));
#2358=CARTESIAN_POINT('Ctrl Pts',(0.359974322031668,-31.2495064777352,16.5175157252576));
#2359=CARTESIAN_POINT('Ctrl Pts',(1.02933886603347,-31.1972354808515,16.460227032321));
#2360=CARTESIAN_POINT('Ctrl Pts',(1.68709482472536,-30.9779968406706,16.4029168679907));
#2361=CARTESIAN_POINT('Ctrl Pts',(2.25558926993638,-30.6144446736241,16.345628545425));
#2362=CARTESIAN_POINT('Ctrl Pts',(2.82408371514739,-30.2508925065775,16.2883402228593));
#2363=CARTESIAN_POINT('Ctrl Pts',(3.30314935266293,-29.7448544918448,16.2310297714992));
#2364=CARTESIAN_POINT('Ctrl Pts',(3.63471257692326,-29.1532292824978,16.1737418130606));
#2365=CARTESIAN_POINT('Ctrl Pts',(3.96627580118359,-28.5616040731508,16.116453854622));
#2366=CARTESIAN_POINT('Ctrl Pts',(4.15104388235541,-27.8860791480164,16.0591431204344));
#2367=CARTESIAN_POINT('Ctrl Pts',(4.16453313646972,-27.2046141566351,16.0018555199961));
#2368=CARTESIAN_POINT('Ctrl Pts',(4.17802239058402,-26.5231491652539,15.9445679195579));
#2369=CARTESIAN_POINT('Ctrl Pts',(4.02164463287101,-25.836899273559,15.8872569066736));
#2370=CARTESIAN_POINT('Ctrl Pts',(3.71066870296272,-25.2265584765752,15.8299696582473));
#2371=CARTESIAN_POINT('Ctrl Pts',(3.39969277305442,-24.6162176795914,15.7726824098211));
#2372=CARTESIAN_POINT('Ctrl Pts',(2.9359020278153,-24.0821430128742,15.7153711223063));
#2373=CARTESIAN_POINT('Ctrl Pts',(2.37108731035637,-23.6886011908956,15.6580842200089));
#2374=CARTESIAN_POINT('Ctrl Pts',(1.80627259289744,-23.295059368917,15.6007973177115));
#2375=CARTESIAN_POINT('Ctrl Pts',(1.14217129355625,-23.0415308728188,15.5434857595736));
#2376=CARTESIAN_POINT('Ctrl Pts',(0.455146988166719,-22.960408497837,15.4861991976495));
#2377=CARTESIAN_POINT('Ctrl Pts',(-0.231877317222808,-22.8792861228552,
15.4289126357253));
#2378=CARTESIAN_POINT('Ctrl Pts',(-0.940537550161691,-22.9692999005262,
15.3716008109));
#2379=CARTESIAN_POINT('Ctrl Pts',(-1.58780992646376,-23.222948487497,15.314314583707));
#2380=CARTESIAN_POINT('Ctrl Pts',(-2.23508230276583,-23.4765970744678,15.2570283565139));
#2381=CARTESIAN_POINT('Ctrl Pts',(-2.82042721228882,-23.8921601369938,15.1997162688729));
#2382=CARTESIAN_POINT('Ctrl Pts',(-3.27383488069023,-24.4236298117793,15.1424303708841));
#2383=CARTESIAN_POINT('Ctrl Pts',(-3.72724254909164,-24.9550994865649,15.0851444728953));
#2384=CARTESIAN_POINT('Ctrl Pts',(-4.04904226418634,-25.6007082903028,15.0278321262568));
#2385=CARTESIAN_POINT('Ctrl Pts',(-4.19901202895418,-26.286500160906,14.9705465520439));
#2386=CARTESIAN_POINT('Ctrl Pts',(-4.34898179372202,-26.9722920315092,14.913260977831));
#2387=CARTESIAN_POINT('Ctrl Pts',(-4.32823823833014,-27.696864249156,14.8559483759565));
#2388=CARTESIAN_POINT('Ctrl Pts',(-4.13620248759561,-28.3756205237803,14.7986631202052));
#2389=CARTESIAN_POINT('Ctrl Pts',(-3.94416673686108,-29.0543767984046,14.741377864454));
#2390=CARTESIAN_POINT('Ctrl Pts',(-3.58247834736109,-29.6866038630478,14.684065011041));
#2391=CARTESIAN_POINT('Ctrl Pts',(-3.09072694158133,-30.1970725249799,14.6267800685391));
#2392=CARTESIAN_POINT('Ctrl Pts',(-2.59897553580158,-30.7075411869121,14.5694951260371));
#2393=CARTESIAN_POINT('Ctrl Pts',(-1.97893887953295,-31.0963900092535,14.5121820247212));
#2394=CARTESIAN_POINT('Ctrl Pts',(-1.30135473340561,-31.3157317897317,14.454897390364));
#2395=CARTESIAN_POINT('Ctrl Pts',(-0.62377058727827,-31.5350735702099,14.3976127560067));
#2396=CARTESIAN_POINT('Ctrl Pts',(0.109859887125027,-31.5858618602476,14.3402994103674));
#2397=CARTESIAN_POINT('Ctrl Pts',(0.814164285621345,-31.4591997061404,14.2830150791426));
#2398=CARTESIAN_POINT('Ctrl Pts',(1.51846868411766,-31.3325375520331,14.2257307479178));
#2399=CARTESIAN_POINT('Ctrl Pts',(2.19257064211805,-31.0299670824768,14.1684171614822));
#2400=CARTESIAN_POINT('Ctrl Pts',(2.75661519721351,-30.5840723334676,14.1111331284776));
#2401=CARTESIAN_POINT('Ctrl Pts',(3.32065975230897,-30.1381775844583,14.0538490954731));
#2402=CARTESIAN_POINT('Ctrl Pts',(3.77459621319051,-29.5507269915758,13.9965352717156));
#2403=CARTESIAN_POINT('Ctrl Pts',(4.0631208515963,-28.8884386652024,13.9392515321084));
#2404=CARTESIAN_POINT('Ctrl Pts',(4.35164549000209,-28.2261503388289,13.8819677925012));
#2405=CARTESIAN_POINT('Ctrl Pts',(4.47554085920862,-27.4906059318028,13.8246537348364));
#2406=CARTESIAN_POINT('Ctrl Pts',(4.4174335988385,-26.7671259696974,13.7673702839072));
#2407=CARTESIAN_POINT('Ctrl Pts',(4.35932633846837,-26.043646007592,13.7100868329779));
#2408=CARTESIAN_POINT('Ctrl Pts',(4.1206457473642,-25.3332578752253,13.6527725447744));
#2409=CARTESIAN_POINT('Ctrl Pts',(3.7264385223253,-24.7197831016981,13.5954893778756));
#2410=CARTESIAN_POINT('Ctrl Pts',(3.33223129728641,-24.106308328171,13.5382062109767));
#2411=CARTESIAN_POINT('Ctrl Pts',(2.78423731477771,-23.5899834651597,13.4808916955503));
#2412=CARTESIAN_POINT('Ctrl Pts',(2.14437202897003,-23.2331957327427,13.4236088081416));
#2413=CARTESIAN_POINT('Ctrl Pts',(1.50450674316235,-22.8764080003258,13.3663259207328));
#2414=CARTESIAN_POINT('Ctrl Pts',(0.774413779611077,-22.6785518889991,13.309011181339));
#2415=CARTESIAN_POINT('Ctrl Pts',(0.0385102376730604,-22.6655520556921,
13.2517285689561));
#2416=CARTESIAN_POINT('Ctrl Pts',(-0.697393304264956,-22.6525522223851,
13.1944459565731));
#2417=CARTESIAN_POINT('Ctrl Pts',(-1.43794247925328,-22.8231062186778,13.1371309964266));
#2418=CARTESIAN_POINT('Ctrl Pts',(-2.09606865842699,-23.160173591663,13.0798486546897));
#2419=CARTESIAN_POINT('Ctrl Pts',(-2.7541948376007,-23.4972409646481,13.0225663129528));
#2420=CARTESIAN_POINT('Ctrl Pts',(-3.32948087019844,-23.9991290609593,12.9652511352145));
#2421=CARTESIAN_POINT('Ctrl Pts',(-3.75287216465629,-24.6094808219334,12.90796905983));
#2422=CARTESIAN_POINT('Ctrl Pts',(-4.17626345911414,-25.2198325829076,12.8506869844455));
#2423=CARTESIAN_POINT('Ctrl Pts',(-4.4481843446811,-25.936961310921,12.7933715922294));
#2424=CARTESIAN_POINT('Ctrl Pts',(-4.53417049873509,-26.6782199281101,12.7360897789783));
#2425=CARTESIAN_POINT('Ctrl Pts',(-4.62015665278908,-27.4194785452993,12.6788079657272));
#2426=CARTESIAN_POINT('Ctrl Pts',(-4.52137115313414,-28.183579240772,12.621492362104));
#2427=CARTESIAN_POINT('Ctrl Pts',(-4.24644889433759,-28.880979930796,12.5642108068469));
#2428=CARTESIAN_POINT('Ctrl Pts',(-3.97152663554103,-29.5783806208201,12.5069292515898));
#2429=CARTESIAN_POINT('Ctrl Pts',(-3.52209512277329,-30.2084906103522,12.4496134395774));
#2430=CARTESIAN_POINT('Ctrl Pts',(-2.94823339092475,-30.6960849276681,12.3923321382562));
#2431=CARTESIAN_POINT('Ctrl Pts',(-2.3743716590762,-31.183679244984,12.335050836935));
#2432=CARTESIAN_POINT('Ctrl Pts',(-1.67779038310626,-31.5289988293348,12.277734819509));
#2433=CARTESIAN_POINT('Ctrl Pts',(-0.938493858503428,-31.6891400501335,
12.2204537681324));
#2434=CARTESIAN_POINT('Ctrl Pts',(-0.199197333900594,-31.8492812709321,
12.1631727167557));
#2435=CARTESIAN_POINT('Ctrl Pts',(0.581419535730098,-31.8252569197531,12.1058564968451));
#2436=CARTESIAN_POINT('Ctrl Pts',(1.31216220335129,-31.616972751076,12.0485756915042));
#2437=CARTESIAN_POINT('Ctrl Pts',(2.04290487097248,-31.408688582399,11.9912948861633));
#2438=CARTESIAN_POINT('Ctrl Pts',(2.72301785637377,-31.017689933097,11.9339784666505));
#2439=CARTESIAN_POINT('Ctrl Pts',(3.27168051216991,-30.4871029608809,11.876697903501));
#2440=CARTESIAN_POINT('Ctrl Pts',(3.82034316796606,-29.9565159886648,11.8194173403514));
#2441=CARTESIAN_POINT('Ctrl Pts',(4.23761275995297,-29.2880562452814,11.7621007240815));
#2442=CARTESIAN_POINT('Ctrl Pts',(4.47233672055251,-28.5582154839675,11.7048203993499));
#2443=CARTESIAN_POINT('Ctrl Pts',(4.70706068115206,-27.8283747226536,11.6475400746183));
#2444=CARTESIAN_POINT('Ctrl Pts',(4.76009229327592,-27.0386382546772,11.5902232643864));
#2445=CARTESIAN_POINT('Ctrl Pts',(4.62236578380915,-26.2809922687663,11.5329431743735));
#2446=CARTESIAN_POINT('Ctrl Pts',(4.48463927434238,-25.5233462828554,11.4756630843606));
#2447=CARTESIAN_POINT('Ctrl Pts',(4.15760185288866,-24.7987006850272,11.4183460829245));
#2448=CARTESIAN_POINT('Ctrl Pts',(3.67680510493408,-24.1928234664463,11.3610662239878));
#2449=CARTESIAN_POINT('Ctrl Pts',(3.19600835697949,-23.5869462478655,11.3037863650511));
#2450=CARTESIAN_POINT('Ctrl Pts',(2.56315379146771,-23.099962191222,11.2464691751292));
#2451=CARTESIAN_POINT('Ctrl Pts',(1.85036321530309,-22.7909920845649,11.1891895436994));
#2452=CARTESIAN_POINT('Ctrl Pts',(1.13757263913847,-22.4820219779078,11.1319099122695));
#2453=CARTESIAN_POINT('Ctrl Pts',(0.346404347142174,-22.3503795041057,11.0745925365344));
#2454=CARTESIAN_POINT('Ctrl Pts',(-0.431256349503487,-22.4142584519129,
11.0173131291038));
#2455=CARTESIAN_POINT('Ctrl Pts',(-1.76387591167286,-22.5237230755283,10.9191576492385));
#2456=CARTESIAN_POINT('Ctrl Pts',(-3.04213419140331,-23.2249589278969,10.8209586709532));
#2457=CARTESIAN_POINT('Ctrl Pts',(-3.85596064138987,-24.2984448521308,10.7227780560402));
#2458=CARTESIAN_POINT('Ctrl Pts',(-4.26287386638314,-24.8351878142477,10.6736877485838));
#2459=CARTESIAN_POINT('Ctrl Pts',(-4.55417709738229,-25.4602183705301,10.6246080237907));
#2460=CARTESIAN_POINT('Ctrl Pts',(-4.70671246799434,-26.1188931345382,10.5755144999941));
#2461=CARTESIAN_POINT('Ctrl Pts',(-4.78211921639114,-26.444512838385,10.5512448307234));
#2462=CARTESIAN_POINT('Ctrl Pts',(-4.82402156275938,-26.7781833518283,10.5269769370843));
#2463=CARTESIAN_POINT('Ctrl Pts',(-4.83034694125566,-27.1129561266807,10.5027146395677));
#2464=CARTESIAN_POINT('Ctrl Pts',(-3.50000130290148,-27.2127226059667,0.497516610448255));
#2465=CARTESIAN_POINT('Ctrl Pts',(-3.51517971121378,-26.6400362227171,0.554808277114941));
#2466=CARTESIAN_POINT('Ctrl Pts',(-3.38700359289755,-26.0622729395371,0.612099943781561));
#2467=CARTESIAN_POINT('Ctrl Pts',(-2.87059541238073,-25.0317435939839,0.72668327711495));
#2468=CARTESIAN_POINT('Ctrl Pts',(-2.48281014130459,-24.5799885832371,0.783974943781635));
#2469=CARTESIAN_POINT('Ctrl Pts',(-1.53584837306688,-23.9107391275463,0.898558277114875));
#2470=CARTESIAN_POINT('Ctrl Pts',(-0.977548004253359,-23.6939293925514,
0.955849943781558));
#2471=CARTESIAN_POINT('Ctrl Pts',(0.179952606081418,-23.5494218341822,1.07043327711495));
#2472=CARTESIAN_POINT('Ctrl Pts',(0.778050826506515,-23.6219155146099,1.1277249437816));
#2473=CARTESIAN_POINT('Ctrl Pts',(1.87337605723642,-24.0427561003574,1.24230827711491));
#2474=CARTESIAN_POINT('Ctrl Pts',(2.36953479367315,-24.3907498795612,1.29959994378166));
#2475=CARTESIAN_POINT('Ctrl Pts',(3.14152373336449,-25.2835693957278,1.41418327711485));
#2476=CARTESIAN_POINT('Ctrl Pts',(3.41657407444237,-25.8275750154296,1.47147494378145));
#2477=CARTESIAN_POINT('Ctrl Pts',(3.67788264996072,-26.9856580353439,1.58605827711506));
#2478=CARTESIAN_POINT('Ctrl Pts',(3.66383841906194,-27.5986380524938,1.64334994378159));
#2479=CARTESIAN_POINT('Ctrl Pts',(3.34637070640969,-28.7497648633494,1.75793327711492));
#2480=CARTESIAN_POINT('Ctrl Pts',(3.04319969463925,-29.2867949482463,1.81522494378156));
#2481=CARTESIAN_POINT('Ctrl Pts',(2.21569737033779,-30.1572282923719,1.92980827711495));
#2482=CARTESIAN_POINT('Ctrl Pts',(1.69211980095435,-30.4897610442556,1.98709994378157));
#2483=CARTESIAN_POINT('Ctrl Pts',(0.545399706903326,-30.8693375696566,2.10168327711494));
#2484=CARTESIAN_POINT('Ctrl Pts',(-0.0766613991650282,-30.9159670184662,
2.1589749437815));
#2485=CARTESIAN_POINT('Ctrl Pts',(-1.27368280615195,-30.7088161970159,2.27355827711501));
#2486=CARTESIAN_POINT('Ctrl Pts',(-1.84748758998441,-30.4551815910792,2.33084994378156));
#2487=CARTESIAN_POINT('Ctrl Pts',(-2.81085451659558,-29.7038376853842,2.44543327711495));
#2488=CARTESIAN_POINT('Ctrl Pts',(-3.19946114294195,-29.2068057482841,2.50272494378152));
#2489=CARTESIAN_POINT('Ctrl Pts',(-3.69753671927098,-28.0836711179268,2.61730827711499));
#2490=CARTESIAN_POINT('Ctrl Pts',(-3.806479757265,-27.4586223362847,2.67459994378158));
#2491=CARTESIAN_POINT('Ctrl Pts',(-3.71562427983475,-26.2264419408016,2.78918327711493));
#2492=CARTESIAN_POINT('Ctrl Pts',(-3.51585940949974,-25.6204942820667,2.84647494378164));
#2493=CARTESIAN_POINT('Ctrl Pts',(-2.85104937088523,-24.5708949233056,2.96105827711487));
#2494=CARTESIAN_POINT('Ctrl Pts',(-2.38659565795852,-24.1282770115141,3.01834994378155));
#2495=CARTESIAN_POINT('Ctrl Pts',(-1.29941716743804,-23.5127467708991,3.13293327711496));
#2496=CARTESIAN_POINT('Ctrl Pts',(-0.677707157851868,-23.3404704661548,
3.19022494378159));
#2497=CARTESIAN_POINT('Ctrl Pts',(0.578163753723292,-23.3101136508809,3.30480827711492));
#2498=CARTESIAN_POINT('Ctrl Pts',(1.21112328389688,-23.4521157051967,3.36209994378163));
#2499=CARTESIAN_POINT('Ctrl Pts',(2.33910331776924,-24.020612363763,3.47668327711488));
#2500=CARTESIAN_POINT('Ctrl Pts',(2.83301955876491,-24.4466103465917,3.53397494378134));
#2501=CARTESIAN_POINT('Ctrl Pts',(3.56365851013518,-25.4854479877254,3.64855827711517));
#2502=CARTESIAN_POINT('Ctrl Pts',(3.79963778298962,-26.0973236259647,3.70584994378171));
#2503=CARTESIAN_POINT('Ctrl Pts',(3.95497605633098,-27.3647903302184,3.8204332771148));
#2504=CARTESIAN_POINT('Ctrl Pts',(3.87413319178915,-28.0191741775874,3.87772494378131));
#2505=CARTESIAN_POINT('Ctrl Pts',(3.41100678604432,-29.2165864086031,3.9923082771152));
#2506=CARTESIAN_POINT('Ctrl Pts',(3.02911682295908,-29.7584488581732,4.04959994378164));
#2507=CARTESIAN_POINT('Ctrl Pts',(2.05088106415332,-30.6005370966614,4.16418327711487));
#2508=CARTESIAN_POINT('Ctrl Pts',(1.45543709786498,-30.8999159637434,4.2214749437816));
#2509=CARTESIAN_POINT('Ctrl Pts',(0.188979096554336,-31.1827816634333,4.33605827711491));
#2510=CARTESIAN_POINT('Ctrl Pts',(-0.480833880026034,-31.1659454082194,
4.39334994378137));
#2511=CARTESIAN_POINT('Ctrl Pts',(-1.73770084949707,-30.8164017691893,4.50793327711514));
#2512=CARTESIAN_POINT('Ctrl Pts',(-2.32353697868073,-30.4839775401827,4.5652249437816));
#2513=CARTESIAN_POINT('Ctrl Pts',(-3.2721043301499,-29.5783412086159,4.67980827711491));
#2514=CARTESIAN_POINT('Ctrl Pts',(-3.63389029917657,-29.0059575948908,4.73709994378148));
#2515=CARTESIAN_POINT('Ctrl Pts',(-4.04554275106343,-27.7534973422558,4.85168327711503));
#2516=CARTESIAN_POINT('Ctrl Pts',(-4.09496422407853,-27.0746032767544,4.90897494378134));
#2517=CARTESIAN_POINT('Ctrl Pts',(-3.86625627856773,-25.7692068883448,5.02355827711517));
#2518=CARTESIAN_POINT('Ctrl Pts',(-3.58829314652568,-25.1439637579671,5.08084994378156));
#2519=CARTESIAN_POINT('Ctrl Pts',(-2.76684994212521,-24.0951805886606,5.19543327711495));
#2520=CARTESIAN_POINT('Ctrl Pts',(-2.22411429181341,-23.6726777785058,5.25272494378155));
#2521=CARTESIAN_POINT('Ctrl Pts',(-0.998892661235347,-23.1323163820897,
5.36730827711496));
#2522=CARTESIAN_POINT('Ctrl Pts',(-0.317558252613747,-23.0150241600847,
5.42459994378155));
#2523=CARTESIAN_POINT('Ctrl Pts',(1.02458823678216,-23.1167103523708,5.53918327711497));
#2524=CARTESIAN_POINT('Ctrl Pts',(1.68411116492473,-23.3356447606771,5.59647494378161));
#2525=CARTESIAN_POINT('Ctrl Pts',(2.82558639662397,-24.061844294864,5.7110582771149));
#2526=CARTESIAN_POINT('Ctrl Pts',(3.30641702010581,-24.568459238132,5.76834994378167));
#2527=CARTESIAN_POINT('Ctrl Pts',(3.97403573885252,-25.7530884168939,5.88293327711484));
#2528=CARTESIAN_POINT('Ctrl Pts',(4.16013798020538,-26.4299946596524,5.94022494378164));
#2529=CARTESIAN_POINT('Ctrl Pts',(4.19049479552954,-27.7963637440239,6.05480827711487));
#2530=CARTESIAN_POINT('Ctrl Pts',(4.03466680450649,-28.4845195073438,6.11209994378139));
#2531=CARTESIAN_POINT('Ctrl Pts',(3.41408166790506,-29.7099502295094,6.22668327711512));
#2532=CARTESIAN_POINT('Ctrl Pts',(2.94987097329771,-30.2460277007815,6.28397494378131));
#2533=CARTESIAN_POINT('Ctrl Pts',(1.8191574593059,-31.0380561478021,6.3985582771152));
#2534=CARTESIAN_POINT('Ctrl Pts',(1.15370655160782,-31.2932049585382,6.45584994378166));
#2535=CARTESIAN_POINT('Ctrl Pts',(-0.22372624653663,-31.4593739468365,6.57043327711484));
#2536=CARTESIAN_POINT('Ctrl Pts',(-0.934395720889725,-31.3701818981879,
6.62772494378144));
#2537=CARTESIAN_POINT('Ctrl Pts',(-2.23389495213891,-30.8647696724464,6.74230827711507));
#2538=CARTESIAN_POINT('Ctrl Pts',(-2.82146111488582,-30.4489835254622,6.79959994378158));
#2539=CARTESIAN_POINT('Ctrl Pts',(-3.73364865213651,-29.3853315240515,6.91418327711493));
#2540=CARTESIAN_POINT('Ctrl Pts',(-4.05735604524484,-28.7384492111523,6.97147494378131));
#2541=CARTESIAN_POINT('Ctrl Pts',(-4.36177886909609,-27.3636162284599,7.0860582771152));
#2542=CARTESIAN_POINT('Ctrl Pts',(-4.34215058957306,-26.6369702924209,7.14334994378177));
#2543=CARTESIAN_POINT('Ctrl Pts',(-3.96053102416322,-25.2743631643761,7.25793327711474));
#2544=CARTESIAN_POINT('Ctrl Pts',(-3.59885357791486,-24.6397209908769,7.31522494378181));
#2545=CARTESIAN_POINT('Ctrl Pts',(-2.61508323909598,-23.61301963208,7.4298082771147));
#2546=CARTESIAN_POINT('Ctrl Pts',(-1.9938935810033,-23.2219804458925,7.48709994378137));
#2547=CARTESIAN_POINT('Ctrl Pts',(-0.635693169822906,-22.7782520675398,
7.60168327711514));
#2548=CARTESIAN_POINT('Ctrl Pts',(0.100033855150708,-22.726038570305,7.65897494378174));
#2549=CARTESIAN_POINT('Ctrl Pts',(1.51380522494329,-22.9763036398845,7.77355827711478));
#2550=CARTESIAN_POINT('Ctrl Pts',(2.19048670189786,-23.2785952980398,7.8308499437815));
#2551=CARTESIAN_POINT('Ctrl Pts',(3.32468611387601,-24.1701378011219,7.94543327711501));
#2552=CARTESIAN_POINT('Ctrl Pts',(3.78108510785602,-24.7585771646693,8.00272494378146));
#2553=CARTESIAN_POINT('Ctrl Pts',(4.36373232434941,-26.085885795444,8.11730827711505));
#2554=CARTESIAN_POINT('Ctrl Pts',(4.48937373037522,-26.8235058310766,8.17459994378218));
#2555=CARTESIAN_POINT('Ctrl Pts',(4.37685682322345,-28.2756184143465,8.28918327711433));
#2556=CARTESIAN_POINT('Ctrl Pts',(4.13875287694128,-28.9887166119371,8.3464749437818));
#2557=CARTESIAN_POINT('Ctrl Pts',(3.35116384720094,-30.2220677165326,8.46105827711471));
#2558=CARTESIAN_POINT('Ctrl Pts',(2.80238767357428,-30.741111051742,8.51834994378256));
#2559=CARTESIAN_POINT('Ctrl Pts',(1.52030780658665,-31.4608182485878,8.63293327711395));
#2560=CARTESIAN_POINT('Ctrl Pts',(0.788205330640013,-31.6607464265703,8.69022494378047));
#2561=CARTESIAN_POINT('Ctrl Pts',(-0.688661926511778,-31.6911032419353,
8.80480827711605));
#2562=CARTESIAN_POINT('Ctrl Pts',(-1.43201392300667,-31.5214493142069,8.86209994378189));
#2563=CARTESIAN_POINT('Ctrl Pts',(-2.75489533342443,-30.8487756995759,8.97668327711462));
#2564=CARTESIAN_POINT('Ctrl Pts',(-3.33313403500641,-30.3463522931823,9.03397494378135));
#2565=CARTESIAN_POINT('Ctrl Pts',(-4.18655197765132,-29.123762906342,9.14855827711516));
#2566=CARTESIAN_POINT('Ctrl Pts',(-4.46087032628663,-28.4047367291627,9.20584994378135));
#2567=CARTESIAN_POINT('Ctrl Pts',(-4.63787002953295,-26.9173378371627,9.32043327711516));
#2568=CARTESIAN_POINT('Ctrl Pts',(-4.54032879677263,-26.1503827357956,9.37772494378163));
#2569=CARTESIAN_POINT('Ctrl Pts',(-3.99263075105309,-24.7487965043376,9.49230827711489));
#2570=CARTESIAN_POINT('Ctrl Pts',(-3.54294842016277,-24.1155266283949,9.54959994378147));
#2571=CARTESIAN_POINT('Ctrl Pts',(-2.393880176143,-23.1332397923951,9.66418327711504));
#2572=CARTESIAN_POINT('Ctrl Pts',(-1.69555951661787,-22.7852038732428,9.72147494378146));
#2573=CARTESIAN_POINT('Ctrl Pts',(-0.21235155257781,-22.4592239252521,9.83605827711505));
#2574=CARTESIAN_POINT('Ctrl Pts',(0.571127342942618,-22.4816442290709,9.8933499437812));
#2575=CARTESIAN_POINT('Ctrl Pts',(2.03947462954967,-22.8953397208652,10.0079332771153));
#2576=CARTESIAN_POINT('Ctrl Pts',(2.72292284739241,-23.2862703843579,10.0652249437816));
#2577=CARTESIAN_POINT('Ctrl Pts',(3.82775821347252,-24.3481747304191,10.179808277115));
#2578=CARTESIAN_POINT('Ctrl Pts',(4.24805061685128,-25.0181704328983,10.237099943781));
#2579=CARTESIAN_POINT('Ctrl Pts',(4.72385492165356,-26.4821110025959,10.3516832771155));
#2580=CARTESIAN_POINT('Ctrl Pts',(4.77886044311237,-27.2746709870712,10.4089749437799));
#2581=CARTESIAN_POINT('Ctrl Pts',(4.50703824947158,-28.796817338216,10.5235582771166));
#2582=CARTESIAN_POINT('Ctrl Pts',(4.18041806520056,-29.5249371617849,10.580849943781));
#2583=CARTESIAN_POINT('Ctrl Pts',(3.21877626343458,-30.7445528163907,10.6954332771156));
#2584=CARTESIAN_POINT('Ctrl Pts',(2.58463318663832,-31.2348479942316,10.752724943781));
#2585=CARTESIAN_POINT('Ctrl Pts',(1.15523755569548,-31.8597810307748,10.8673082771155));
#2586=CARTESIAN_POINT('Ctrl Pts',(0.361331893025007,-31.9937716208391,10.9245999437816));
#2587=CARTESIAN_POINT('Ctrl Pts',(-1.20074678409337,-31.8704239988137,11.0391832771149));
#2588=CARTESIAN_POINT('Ctrl Pts',(-1.96742025115454,-31.6131505145616,11.0964749437817));
#2589=CARTESIAN_POINT('Ctrl Pts',(-3.29264722862687,-30.7641719892639,11.2110582771148));
#2590=CARTESIAN_POINT('Ctrl Pts',(-3.84990327557803,-30.1732345852601,11.2683499437819));
#2591=CARTESIAN_POINT('Ctrl Pts',(-4.62169895051392,-28.7937040300877,11.3829332771146));
#2592=CARTESIAN_POINT('Ctrl Pts',(-4.83545306471002,-28.0064053323945,11.4402249437801));
#2593=CARTESIAN_POINT('Ctrl Pts',(-4.85063147283344,-27.2127226059663,11.4975166104483));
#2594=CARTESIAN_POINT('Ctrl Pts',(-2.50007468503219,-27.2005618150104,0.498733179016744));
#2595=CARTESIAN_POINT('Ctrl Pts',(-2.51326328854572,-26.7914880446566,0.55602484568343));
#2596=CARTESIAN_POINT('Ctrl Pts',(-2.424042889801,-26.3776787977216,0.613316512350049));
#2597=CARTESIAN_POINT('Ctrl Pts',(-2.05837790695547,-25.6376123049861,0.727899845683439));
#2598=CARTESIAN_POINT('Ctrl Pts',(-1.78223591282738,-25.3120882495965,0.785191512350124));
#2599=CARTESIAN_POINT('Ctrl Pts',(-1.10514101707629,-24.8279443088378,0.899774845683364));
#2600=CARTESIAN_POINT('Ctrl Pts',(-0.704806088645041,-24.6698320611445,
0.957066512350047));
#2601=CARTESIAN_POINT('Ctrl Pts',(0.127435052567004,-24.5613586294748,1.07164984568344));
#2602=CARTESIAN_POINT('Ctrl Pts',(0.558550388136447,-24.611154478993,1.12894151235009));
#2603=CARTESIAN_POINT('Ctrl Pts',(1.35003600685502,-24.9104480749466,1.2435248456834));
#2604=CARTESIAN_POINT('Ctrl Pts',(1.70962866979797,-25.1597089674028,1.30081651235015));
#2605=CARTESIAN_POINT('Ctrl Pts',(2.27095184904808,-25.8021046070125,1.41539984568334));
#2606=CARTESIAN_POINT('Ctrl Pts',(2.47210402656363,-26.1946587930152,1.47269151234994));
#2607=CARTESIAN_POINT('Ctrl Pts',(2.66567098650756,-27.0325805190397,1.58727484568355));
#2608=CARTESIAN_POINT('Ctrl Pts',(2.65784810539905,-27.4771569431548,1.64456651235008));
#2609=CARTESIAN_POINT('Ctrl Pts',(2.43156061069391,-28.3139935243568,1.75914984568341));
#2610=CARTESIAN_POINT('Ctrl Pts',(2.21326124381233,-28.7054376235712,1.81644151235005));
#2611=CARTESIAN_POINT('Ctrl Pts',(1.61432808129647,-29.341673788178,1.93102484568344));
#2612=CARTESIAN_POINT('Ctrl Pts',(1.23422937884041,-29.5858193799578,1.98831651235005));
#2613=CARTESIAN_POINT('Ctrl Pts',(0.399489075163559,-29.8665991896874,2.10289984568343));
#2614=CARTESIAN_POINT('Ctrl Pts',(-0.0543695483476922,-29.902913592182,
2.16019151234999));
#2615=CARTESIAN_POINT('Ctrl Pts',(-0.929676894760097,-29.7556981014736,
2.2747748456835));
#2616=CARTESIAN_POINT('Ctrl Pts',(-1.35027785335415,-29.5722565382445,2.33206651235005));
#2617=CARTESIAN_POINT('Ctrl Pts',(-2.05817162822115,-29.0254258335761,2.44664984568344));
#2618=CARTESIAN_POINT('Ctrl Pts',(-2.34475331460298,-28.6625184167178,2.50394151235001));
#2619=CARTESIAN_POINT('Ctrl Pts',(-2.71392854153148,-27.8401775372868,2.61852484568348));
#2620=CARTESIAN_POINT('Ctrl Pts',(-2.79611947665046,-27.38151024587,2.67581651235007));
#2621=CARTESIAN_POINT('Ctrl Pts',(-2.73337723274891,-26.4753694596141,2.79039984568342));
#2622=CARTESIAN_POINT('Ctrl Pts',(-2.58845080557611,-26.0287680290841,2.84769151235013));
#2623=CARTESIAN_POINT('Ctrl Pts',(-2.10212843329669,-25.253457448189,2.96227484568336));
#2624=CARTESIAN_POINT('Ctrl Pts',(-1.76115320148598,-24.925519700272,3.01956651235004));
#2625=CARTESIAN_POINT('Ctrl Pts',(-0.960685614181144,-24.4677520619668,
3.13414984568345));
#2626=CARTESIAN_POINT('Ctrl Pts',(-0.501933757791044,-24.3384072792704,
3.19144151235008));
#2627=CARTESIAN_POINT('Ctrl Pts',(0.426711935575103,-24.3120300735039,3.30602484568341));
#2628=CARTESIAN_POINT('Ctrl Pts',(0.895717425864195,-24.4150764083739,3.36331651235012));
#2629=CARTESIAN_POINT('Ctrl Pts',(1.73323460661518,-24.8328298691077,3.47789984568337));
#2630=CARTESIAN_POINT('Ctrl Pts',(2.10091989250226,-25.1471845752111,3.53519151234975));
#2631=CARTESIAN_POINT('Ctrl Pts',(2.64645332874688,-25.9161553435738,3.64977484568374));
#2632=CARTESIAN_POINT('Ctrl Pts',(2.82373511441566,-26.3700655417409,3.70706651235029));
#2633=CARTESIAN_POINT('Ctrl Pts',(2.94303926101928,-27.3122727765361,3.8216498456832));
#2634=CARTESIAN_POINT('Ctrl Pts',(2.88489422734382,-27.7996737393716,3.8789415123498));
#2635=CARTESIAN_POINT('Ctrl Pts',(2.54331481151743,-28.6932463580673,3.99352484568369));
#2636=CARTESIAN_POINT('Ctrl Pts',(2.26015773499116,-29.0985427344035,4.05081651235013));
#2637=CARTESIAN_POINT('Ctrl Pts',(1.53234585299496,-29.7299652122396,4.16539984568336));
#2638=CARTESIAN_POINT('Ctrl Pts',(1.08835332012082,-29.9554459158982,4.22269151235009));
#2639=CARTESIAN_POINT('Ctrl Pts',(0.142056613017233,-30.1705699999466,4.3372748456834));
#2640=CARTESIAN_POINT('Ctrl Pts',(-0.359352770840531,-30.1599550945101,
4.39456651234986));
#2641=CARTESIAN_POINT('Ctrl Pts',(-1.30192951035091,-29.9015916735199,4.50914984568362));
#2642=CARTESIAN_POINT('Ctrl Pts',(-1.74217965412023,-29.6540390892461,4.56644151235009));
#2643=CARTESIAN_POINT('Ctrl Pts',(-2.45654982584139,-28.9769719196844,4.6810248456834));
#2644=CARTESIAN_POINT('Ctrl Pts',(-2.72994863492545,-28.5480671726279,4.73831651234997));
#2645=CARTESIAN_POINT('Ctrl Pts',(-3.04280437104754,-27.607586710665,4.85289984568352));
#2646=CARTESIAN_POINT('Ctrl Pts',(-3.08191079776549,-27.0968951274201,4.91019151234983));
#2647=CARTESIAN_POINT('Ctrl Pts',(-2.91313818305431,-26.1132127998883,5.02477484568366));
#2648=CARTESIAN_POINT('Ctrl Pts',(-2.7053680935962,-25.641173494479,5.08206651235005));
#2649=CARTESIAN_POINT('Ctrl Pts',(-2.08843809041187,-24.8478634771535,5.19664984568344));
#2650=CARTESIAN_POINT('Ctrl Pts',(-1.67982696010923,-24.527385606786,5.25394151235004));
#2651=CARTESIAN_POINT('Ctrl Pts',(-0.755399080733289,-24.115924559888,5.36852484568345));
#2652=CARTESIAN_POINT('Ctrl Pts',(-0.240446162052198,-24.025384440712,5.42581651235003));
#2653=CARTESIAN_POINT('Ctrl Pts',(0.775660717822627,-24.0989573994438,5.54039984568345));
#2654=CARTESIAN_POINT('Ctrl Pts',(1.27583741803011,-24.2630533646806,5.5976915123501));
#2655=CARTESIAN_POINT('Ctrl Pts',(2.14302387161775,-24.8107652323726,5.71227484568339));
#2656=CARTESIAN_POINT('Ctrl Pts',(2.50917433141652,-25.1939016947322,5.76956651235015));
#2657=CARTESIAN_POINT('Ctrl Pts',(3.01903044771613,-26.0918199700231,5.88414984568333));
#2658=CARTESIAN_POINT('Ctrl Pts',(3.16220116709098,-26.605768059855,5.94144151235013));
#2659=CARTESIAN_POINT('Ctrl Pts',(3.18857837290535,-27.6449119257339,6.05602484568335));
#2660=CARTESIAN_POINT('Ctrl Pts',(3.07170610126387,-28.1691136494362,6.11331651234988));
#2661=CARTESIAN_POINT('Ctrl Pts',(2.60186416262591,-29.1040815182302,6.22789984568361));
#2662=CARTESIAN_POINT('Ctrl Pts',(2.24929674456444,-29.5139280345983,6.2851915123498));
#2663=CARTESIAN_POINT('Ctrl Pts',(1.38845010357141,-30.1208509663343,6.39977484568369));
#2664=CARTESIAN_POINT('Ctrl Pts',(0.880964635695304,-30.3173022899789,6.45706651235015));
#2665=CARTESIAN_POINT('Ctrl Pts',(-0.171208692717956,-30.4474371515102,
6.57164984568333));
#2666=CARTESIAN_POINT('Ctrl Pts',(-0.714895282800354,-30.3809429336921,
6.62894151234993));
#2667=CARTESIAN_POINT('Ctrl Pts',(-1.71055490147675,-29.99707769797,6.74352484568356));
#2668=CARTESIAN_POINT('Ctrl Pts',(-2.1615549912013,-29.680024437392,6.80081651235007));
#2669=CARTESIAN_POINT('Ctrl Pts',(-2.8630767676294,-28.8667963129956,6.91539984568342));
#2670=CARTESIAN_POINT('Ctrl Pts',(-3.11288599742707,-28.3713654332789,6.9726915123498));
#2671=CARTESIAN_POINT('Ctrl Pts',(-3.34956720558195,-27.316693745052,7.08727484568369));
#2672=CARTESIAN_POINT('Ctrl Pts',(-3.33616027582943,-26.758451401481,7.14456651235026));
#2673=CARTESIAN_POINT('Ctrl Pts',(-3.0457209285282,-25.7101345036477,7.25914984568322));
#2674=CARTESIAN_POINT('Ctrl Pts',(-2.76891512688693,-25.2210783153451,7.31644151235029));
#2675=CARTESIAN_POINT('Ctrl Pts',(-2.01371395025572,-24.4285741364808,7.43102484568319));
#2676=CARTESIAN_POINT('Ctrl Pts',(-1.53600315861845,-24.1259221101056,7.48831651234986));
#2677=CARTESIAN_POINT('Ctrl Pts',(-0.489782538354123,-23.7809904475937,
7.60289984568363));
#2678=CARTESIAN_POINT('Ctrl Pts',(0.0777420046090931,-23.7390919966418,
7.66019151235023));
#2679=CARTESIAN_POINT('Ctrl Pts',(1.16979931327565,-23.9294217353742,7.77477484568326));
#2680=CARTESIAN_POINT('Ctrl Pts',(1.69327696548401,-24.1615203510483,7.83206651235037));
#2681=CARTESIAN_POINT('Ctrl Pts',(2.57200322528511,-24.8485496527562,7.94664984568312));
#2682=CARTESIAN_POINT('Ctrl Pts',(2.92637727962451,-25.3028644964882,8.00394151234995));
#2683=CARTESIAN_POINT('Ctrl Pts',(3.38012414650242,-26.3293793758314,8.11852484568354));
#2684=CARTESIAN_POINT('Ctrl Pts',(3.47901344973788,-26.9006179217584,8.17581651235106));
#2685=CARTESIAN_POINT('Ctrl Pts',(3.39460977616041,-28.0266908952667,8.29039984568243));
#2686=CARTESIAN_POINT('Ctrl Pts',(3.21134427287294,-28.5804428651419,8.34769151235029));
#2687=CARTESIAN_POINT('Ctrl Pts',(2.60224290975714,-29.539505191427,8.4622748456832));
#2688=CARTESIAN_POINT('Ctrl Pts',(2.17694521686884,-29.9438683631093,8.51956651235105));
#2689=CARTESIAN_POINT('Ctrl Pts',(1.18157625356271,-30.5058129573948,8.63414984568244));
#2690=CARTESIAN_POINT('Ctrl Pts',(0.612431930317692,-30.662809613458,8.69144151234896));
#2691=CARTESIAN_POINT('Ctrl Pts',(-0.537210108102021,-30.689186819309,8.80602484568453));
#2692=CARTESIAN_POINT('Ctrl Pts',(-1.11660806520128,-30.5584886109117,8.86331651235037));
#2693=CARTESIAN_POINT('Ctrl Pts',(-2.149026622043,-30.0365581943494,8.97789984568311));
#2694=CARTESIAN_POINT('Ctrl Pts',(-2.60103436888815,-29.6457780643529,9.03519151234983));
#2695=CARTESIAN_POINT('Ctrl Pts',(-3.2693467961186,-28.6930555507037,9.14977484568365));
#2696=CARTESIAN_POINT('Ctrl Pts',(-3.48496765774055,-28.1319948131383,9.20706651234983));
#2697=CARTESIAN_POINT('Ctrl Pts',(-3.62593323419338,-26.9698553910934,9.32164984568365));
#2698=CARTESIAN_POINT('Ctrl Pts',(-3.55108983223544,-26.3698831737798,9.37894151235011));
#2699=CARTESIAN_POINT('Ctrl Pts',(-3.12493877661809,-25.2721365551049,9.49352484568337));
#2700=CARTESIAN_POINT('Ctrl Pts',(-2.77398933200833,-24.7754327520073,9.55081651234996));
#2701=CARTESIAN_POINT('Ctrl Pts',(-1.87534496517122,-24.0038116769744,9.66539984568352));
#2702=CARTESIAN_POINT('Ctrl Pts',(-1.32847573863619,-23.7296739210376,9.72269151234995));
#2703=CARTESIAN_POINT('Ctrl Pts',(-0.165429069278296,-23.4714355887892,
9.83727484568354));
#2704=CARTESIAN_POINT('Ctrl Pts',(0.449646233987307,-23.4876345428461,9.89456651234969));
#2705=CARTESIAN_POINT('Ctrl Pts',(1.60370329017324,-23.8101498164686,10.0091498456838));
#2706=CARTESIAN_POINT('Ctrl Pts',(2.14156552300047,-24.1162088354615,10.06644151235));
#2707=CARTESIAN_POINT('Ctrl Pts',(3.01220370899539,-24.9495440191837,10.1810248456835));
#2708=CARTESIAN_POINT('Ctrl Pts',(3.34410895267091,-25.4760608553855,10.2383165123495));
#2709=CARTESIAN_POINT('Ctrl Pts',(3.72111654156689,-26.6280216339623,10.352899845684));
#2710=CARTESIAN_POINT('Ctrl Pts',(3.76580701675634,-27.2523791366326,10.4101915123484));
#2711=CARTESIAN_POINT('Ctrl Pts',(3.55392015400117,-28.4528114264453,10.5247748456851));
#2712=CARTESIAN_POINT('Ctrl Pts',(3.29749301212752,-29.0277274254513,10.5820665123494));
#2713=CARTESIAN_POINT('Ctrl Pts',(2.54036441186484,-29.9918699277194,10.696649845684));
#2714=CARTESIAN_POINT('Ctrl Pts',(2.04034585472464,-30.3801401660391,10.7539415123495));
#2715=CARTESIAN_POINT('Ctrl Pts',(0.911743975403001,-30.8761728528888,10.868524845684));
#2716=CARTESIAN_POINT('Ctrl Pts',(0.284219802238695,-30.9834113401931,10.9258165123501));
#2717=CARTESIAN_POINT('Ctrl Pts',(-0.951819264909011,-30.8881769517593,
11.0403998456834));
#2718=CARTESIAN_POINT('Ctrl Pts',(-1.55914650444578,-30.6857419104376,11.0976915123502));
#2719=CARTESIAN_POINT('Ctrl Pts',(-2.61008470343474,-30.0152510518758,11.2122748456833));
#2720=CARTESIAN_POINT('Ctrl Pts',(-3.0526605869948,-29.5477921284695,11.2695665123504));
#2721=CARTESIAN_POINT('Ctrl Pts',(-3.66669365927143,-28.4549724771489,11.3841498456831));
#2722=CARTESIAN_POINT('Ctrl Pts',(-3.83751625162752,-27.8306319296078,11.4414415123486));
#2723=CARTESIAN_POINT('Ctrl Pts',(-3.85070485496414,-27.2005618150101,11.4987331790167));
#2724=CARTESIAN_POINT('Ctrl Pts',(-2.50007468503219,-27.1010184425723,-0.496300045053517));
#2725=CARTESIAN_POINT('Ctrl Pts',(-2.4969755420553,-26.6919446722147,-0.439008378386831));
#2726=CARTESIAN_POINT('Ctrl Pts',(-2.39148297849306,-26.282211390483,-0.381716711720212));
#2727=CARTESIAN_POINT('Ctrl Pts',(-1.99708897638351,-25.5575008784686,-0.267133378386822));
#2728=CARTESIAN_POINT('Ctrl Pts',(-1.70851761043281,-25.2432421490424,-0.209841711720177));
#2729=CARTESIAN_POINT('Ctrl Pts',(-1.01332474089414,-24.78618374015,-0.0952583783868566));
#2730=CARTESIAN_POINT('Ctrl Pts',(-0.607338523048543,-24.6438657882886,
-0.0379667117201735));
#2731=CARTESIAN_POINT('Ctrl Pts',(0.228095574754098,-24.5678109889204,0.0766166216131396));
#2732=CARTESIAN_POINT('Ctrl Pts',(0.656749523111612,-24.6342001631764,0.133908288279827));
#2733=CARTESIAN_POINT('Ctrl Pts',(1.43576904066519,-24.9635895896308,0.248491621613139));
#2734=CARTESIAN_POINT('Ctrl Pts',(1.78536891475194,-25.2263241981206,0.305783288279848));
#2735=CARTESIAN_POINT('Ctrl Pts',(2.32151089800951,-25.8893855112099,0.420366621613118));
#2736=CARTESIAN_POINT('Ctrl Pts',(2.50749875677538,-26.2891118858318,0.477658288279721));
#2737=CARTESIAN_POINT('Ctrl Pts',(2.66911615346284,-27.133388775121,0.592241621613245));
#2738=CARTESIAN_POINT('Ctrl Pts',(2.64453859088259,-27.5771420945141,0.649533288279816));
#2739=CARTESIAN_POINT('Ctrl Pts',(2.38707829372837,-28.404522509479,0.76411662161315));
#2740=CARTESIAN_POINT('Ctrl Pts',(2.15439062586044,-28.7873425929663,0.821408288279792));
#2741=CARTESIAN_POINT('Ctrl Pts',(1.53242311190211,-29.4005444061292,0.935991621613174));
#2742=CARTESIAN_POINT('Ctrl Pts',(1.14370039372121,-29.6303016969254,0.993283288279668));
#2743=CARTESIAN_POINT('Ctrl Pts',(0.299503923801187,-29.8799087042019,1.1078666216133));
#2744=CARTESIAN_POINT('Ctrl Pts',(-0.155177804428747,-29.8994684252318,
1.16515828827989));
#2745=CARTESIAN_POINT('Ctrl Pts',(-1.02412998757692,-29.7203033712568,1.27974162161307));
#2746=CARTESIAN_POINT('Ctrl Pts',(-1.43755875755687,-29.5216974892904,1.33703328827979));
#2747=CARTESIAN_POINT('Ctrl Pts',(-2.12478685893361,-28.9496855886148,1.45161662161318));
#2748=CARTESIAN_POINT('Ctrl Pts',(-2.39789482929683,-28.5767853829115,1.50890828827974));
#2749=CARTESIAN_POINT('Ctrl Pts',(-2.73697422570521,-27.7419784023078,1.62349162161322));
#2750=CARTESIAN_POINT('Ctrl Pts',(-2.80257183610632,-27.280849723684,1.68078328827981));
#2751=CARTESIAN_POINT('Ctrl Pts',(-2.70741095988276,-26.3779018940165,1.79536662161316));
#2752=CARTESIAN_POINT('Ctrl Pts',(-2.54669023689932,-25.9369517528952,1.85265828827987));
#2753=CARTESIAN_POINT('Ctrl Pts',(-2.03328233273154,-25.1797391458012,1.9672416216131));
#2754=CARTESIAN_POINT('Ctrl Pts',(-1.68104177497557,-24.8642307696851,2.02453328827986));
#2755=CARTESIAN_POINT('Ctrl Pts',(-0.865218206935421,-24.4351921506738,
2.1391166216131));
#2756=CARTESIAN_POINT('Ctrl Pts',(-0.402390385352991,-24.3221195331577,
2.19640828827973));
#2757=CARTESIAN_POINT('Ctrl Pts',(0.526255308013156,-24.3283178196167,2.31099162161323));
#2758=CARTESIAN_POINT('Ctrl Pts',(0.991184833112652,-24.4476363196676,2.36828328827977));
#2759=CARTESIAN_POINT('Ctrl Pts',(1.81334603312285,-24.8941187996939,2.4828666216132));
#2760=CARTESIAN_POINT('Ctrl Pts',(2.16976599307112,-25.2209028775953,2.54015828827966));
#2761=CARTESIAN_POINT('Ctrl Pts',(2.68821389741996,-26.0079716197664,2.65474162161331));
#2762=CARTESIAN_POINT('Ctrl Pts',(2.84970138728746,-26.4675331073362,2.71203328827994));
#2763=CARTESIAN_POINT('Ctrl Pts',(2.93658690155775,-27.4129332987244,2.82661662161303));
#2764=CARTESIAN_POINT('Ctrl Pts',(2.86184854317733,-27.8978728743535,2.88390828827962));
#2765=CARTESIAN_POINT('Ctrl Pts',(2.49017329681634,-28.7789793918707,2.99849162161334));
#2766=CARTESIAN_POINT('Ctrl Pts',(2.19354250428536,-29.1742829793717,3.05578328827987));
#2767=CARTESIAN_POINT('Ctrl Pts',(1.44506494878558,-29.7805242611867,3.1703666216131));
#2768=CARTESIAN_POINT('Ctrl Pts',(0.993900227308371,-29.9908406461274,3.22765828827983));
#2769=CARTESIAN_POINT('Ctrl Pts',(0.0412483569317987,-30.1740151668844,
3.34224162161314));
#2770=CARTESIAN_POINT('Ctrl Pts',(-0.459337922206362,-30.1466455800109,
3.3995332882796));
#2771=CARTESIAN_POINT('Ctrl Pts',(-1.39245849546665,-29.8571093565371,3.51411662161336));
#2772=CARTESIAN_POINT('Ctrl Pts',(-1.82408462352403,-29.5951684713072,3.57140828827983));
#2773=CARTESIAN_POINT('Ctrl Pts',(-2.51542044378384,-28.895066950277,3.68599162161314));
#2774=CARTESIAN_POINT('Ctrl Pts',(-2.77443095190869,-28.4575381875142,3.74328328827971));
#2775=CARTESIAN_POINT('Ctrl Pts',(-3.0561138855463,-27.5076015592972,3.85786662161326));
#2776=CARTESIAN_POINT('Ctrl Pts',(-3.07846563082932,-26.9960868713341,3.91515828827957));
#2777=CARTESIAN_POINT('Ctrl Pts',(-2.87774345282345,-26.0187597070765,4.0297416216134));
#2778=CARTESIAN_POINT('Ctrl Pts',(-2.6548090446523,-25.5538925902661,4.0870332882796));
#2779=CARTESIAN_POINT('Ctrl Pts',(-2.01269784544036,-24.7812482464512,4.20161662161336));
#2780=CARTESIAN_POINT('Ctrl Pts',(-1.59409392630807,-24.4742440920755,4.25890828827978));
#2781=CARTESIAN_POINT('Ctrl Pts',(-0.657199945749121,-24.0928788757309,
4.37349162161319));
#2782=CARTESIAN_POINT('Ctrl Pts',(-0.13978563986163,-24.0189320812405,4.43078328827959));
#2783=CARTESIAN_POINT('Ctrl Pts',(0.873128283415644,-24.1249236723256,4.54536662161338));
#2784=CARTESIAN_POINT('Ctrl Pts',(1.36765369423033,-24.3048139333446,4.60265828827984));
#2785=CARTESIAN_POINT('Ctrl Pts',(2.21674217399424,-24.8796113329506,4.71724162161312));
#2786=CARTESIAN_POINT('Ctrl Pts',(2.57046326201523,-25.2740131212371,4.77453328828008));
#2787=CARTESIAN_POINT('Ctrl Pts',(3.05159035899733,-26.1872873772743,4.88911662161288));
#2788=CARTESIAN_POINT('Ctrl Pts',(3.17848891321873,-26.705311432293,4.94640828827969));
#2789=CARTESIAN_POINT('Ctrl Pts',(3.17229062677759,-27.7444552981719,5.06099162161328));
#2790=CARTESIAN_POINT('Ctrl Pts',(3.03914618998225,-28.2645810566892,5.11828328827961));
#2791=CARTESIAN_POINT('Ctrl Pts',(2.54057523202762,-29.1841929447334,5.23286662161335));
#2792=CARTESIAN_POINT('Ctrl Pts',(2.17557844218674,-29.5827741351755,5.29015828827954));
#2793=CARTESIAN_POINT('Ctrl Pts',(1.2966338273724,-30.1626115349991,5.40474162161343));
#2794=CARTESIAN_POINT('Ctrl Pts',(0.783497070102546,-30.3432685628663,5.46203328828008));
#2795=CARTESIAN_POINT('Ctrl Pts',(-0.271869214908782,-30.440984792033,5.57661662161288));
#2796=CARTESIAN_POINT('Ctrl Pts',(-0.813094417788087,-30.3578972495394,
5.63390828827948));
#2797=CARTESIAN_POINT('Ctrl Pts',(-1.79628793527435,-29.9439361832551,5.74849162161349));
#2798=CARTESIAN_POINT('Ctrl Pts',(-2.23729523617899,-29.6134092066964,5.80578328828));
#2799=CARTESIAN_POINT('Ctrl Pts',(-2.9136358165671,-28.7795154087759,5.92036662161297));
#2800=CARTESIAN_POINT('Ctrl Pts',(-3.14828072766742,-28.2769123404668,5.97765828827954));
#2801=CARTESIAN_POINT('Ctrl Pts',(-3.35301237250861,-27.2158854889663,6.09224162161343));
#2802=CARTESIAN_POINT('Ctrl Pts',(-3.32285076134111,-26.6584662501118,6.14953328827981));
#2803=CARTESIAN_POINT('Ctrl Pts',(-3.00123861153452,-25.6196055185354,6.26411662161316));
#2804=CARTESIAN_POINT('Ctrl Pts',(-2.71004450895648,-25.1391733459278,6.32140828828022));
#2805=CARTESIAN_POINT('Ctrl Pts',(-1.93180898083992,-24.3697035185519,6.43599162161274));
#2806=CARTESIAN_POINT('Ctrl Pts',(-1.4454741735086,-24.0814397931112,6.49328328827941));
#2807=CARTESIAN_POINT('Ctrl Pts',(-0.389797386982391,-23.7676809331061,
6.60786662161356));
#2808=CARTESIAN_POINT('Ctrl Pts',(0.178550260697191,-23.7425371635652,6.66515828827996));
#2809=CARTESIAN_POINT('Ctrl Pts',(1.26425240608542,-23.9648164656178,6.779741621613));
#2810=CARTESIAN_POINT('Ctrl Pts',(1.78055786970335,-24.2120793999817,6.83703328828011));
#2811=CARTESIAN_POINT('Ctrl Pts',(2.63861845598095,-24.9242898977382,6.95161662161285));
#2812=CARTESIAN_POINT('Ctrl Pts',(2.97951879434458,-25.3885975302847,7.00890828827969));
#2813=CARTESIAN_POINT('Ctrl Pts',(3.40316983064992,-26.4275785108202,7.12349162161328));
#2814=CARTESIAN_POINT('Ctrl Pts',(3.48546580921967,-27.0012784439486,7.18078328828002));
#2815=CARTESIAN_POINT('Ctrl Pts',(3.36864350326833,-28.12415846086,7.29536662161295));
#2816=CARTESIAN_POINT('Ctrl Pts',(3.16958370421836,-28.6722591413468,7.35265828828003));
#2817=CARTESIAN_POINT('Ctrl Pts',(2.53339680916978,-29.6132234937987,7.46724162161294));
#2818=CARTESIAN_POINT('Ctrl Pts',(2.09683379037026,-30.0051572937212,7.5245332882802));
#2819=CARTESIAN_POINT('Ctrl Pts',(1.08610884630516,-30.5383728686628,7.63911662161277));
#2820=CARTESIAN_POINT('Ctrl Pts',(0.512888557879637,-30.6790973595949,7.6964082882785));
#2821=CARTESIAN_POINT('Ctrl Pts',(-0.636753480540073,-30.6728990731721,
7.81099162161447));
#2822=CARTESIAN_POINT('Ctrl Pts',(-1.21207547246262,-30.5259286996412,7.86828328828011));
#2823=CARTESIAN_POINT('Ctrl Pts',(-2.22913804853779,-29.97526926374,7.98286662161285));
#2824=CARTESIAN_POINT('Ctrl Pts',(-2.66988046947652,-29.5720597619835,8.04015828827957));
#2825=CARTESIAN_POINT('Ctrl Pts',(-3.31110736477216,-28.6012392744964,8.15474162161339));
#2826=CARTESIAN_POINT('Ctrl Pts',(-3.51093393063736,-28.0345272475469,8.21203328827957));
#2827=CARTESIAN_POINT('Ctrl Pts',(-3.61948087470683,-26.8691948689011,8.32661662161339));
#2828=CARTESIAN_POINT('Ctrl Pts',(-3.52804414809214,-26.2716840387888,8.38390828827985));
#2829=CARTESIAN_POINT('Ctrl Pts',(-3.07179726189379,-25.1864035213107,8.49849162161311));
#2830=CARTESIAN_POINT('Ctrl Pts',(-2.70737410131727,-24.69969250702,8.5557832882797));
#2831=CARTESIAN_POINT('Ctrl Pts',(-1.78806406094709,-23.9532526280462,8.67036662161327));
#2832=CARTESIAN_POINT('Ctrl Pts',(-1.23402264582689,-23.6942791907854,8.72765828827969));
#2833=CARTESIAN_POINT('Ctrl Pts',(-0.0646208131897154,-23.4679904218743,
8.84224162161328));
#2834=CARTESIAN_POINT('Ctrl Pts',(0.549631385361328,-23.5009440573235,8.89953328827943));
#2835=CARTESIAN_POINT('Ctrl Pts',(1.69423227528079,-23.8546321334732,9.01411662161354));
#2836=CARTESIAN_POINT('Ctrl Pts',(2.2234704924224,-24.1750794533858,9.07140828827978));
#2837=CARTESIAN_POINT('Ctrl Pts',(3.0710743269197,-25.0314489886056,9.18599162161319));
#2838=CARTESIAN_POINT('Ctrl Pts',(3.38859126967608,-25.566589840493,9.24328328827926));
#2839=CARTESIAN_POINT('Ctrl Pts',(3.73442605604372,-26.7280067853365,9.3578666216137));
#2840=CARTESIAN_POINT('Ctrl Pts',(3.76236184984361,-27.3531873927232,9.41515828827891));
#2841=CARTESIAN_POINT('Ctrl Pts',(3.51852542374687,-28.5472645192526,9.52974162161405));
#2842=CARTESIAN_POINT('Ctrl Pts',(3.24693396320241,-29.1150083296771,9.58703328827918));
#2843=CARTESIAN_POINT('Ctrl Pts',(2.46462416687454,-30.0584851584089,9.70161662161378));
#2844=CARTESIAN_POINT('Ctrl Pts',(1.95461282093448,-30.433281680772,9.75890828827921));
#2845=CARTESIAN_POINT('Ctrl Pts',(0.813544840407825,-30.8992185370235,9.87349162161376));
#2846=CARTESIAN_POINT('Ctrl Pts',(0.183559280048123,-30.9898636996832,9.9307832882798));
#2847=CARTESIAN_POINT('Ctrl Pts',(-1.04928683050202,-30.8622106788589,10.0453666216132));
#2848=CARTESIAN_POINT('Ctrl Pts',(-1.65096278065817,-30.64398134179,10.1026582882799));
#2849=CARTESIAN_POINT('Ctrl Pts',(-2.68380300579906,-29.9464049512814,10.217241621613));
#2850=CARTESIAN_POINT('Ctrl Pts',(-3.11394951761039,-29.4676807019775,10.2745332882801));
#2851=CARTESIAN_POINT('Ctrl Pts',(-3.69925357053573,-28.3595050698848,10.3891166216128));
#2852=CARTESIAN_POINT('Ctrl Pts',(-3.85380399801319,-27.7310885571697,10.4464082882783));
#2853=CARTESIAN_POINT('Ctrl Pts',(-3.85070485496413,-27.101018442572,10.5036999549465));
#2854=CARTESIAN_POINT('Ctrl Pts',(-3.5,-27.1131792176833,-0.497516612035131));
#2855=CARTESIAN_POINT('Ctrl Pts',(-3.49889065922935,-26.5404930476192,-0.440224945368445));
#2856=CARTESIAN_POINT('Ctrl Pts',(-3.3544424268553,-25.9668059432703,-0.382933278701826));
#2857=CARTESIAN_POINT('Ctrl Pts',(-2.80930542349117,-24.951632956913,-0.268349945368436));
#2858=CARTESIAN_POINT('Ctrl Pts',(-2.40909092606461,-24.5111434366068,-0.211058278701791));
#2859=CARTESIAN_POINT('Ctrl Pts',(-1.4440315356738,-23.8689797539743,-0.0964749453684705));
#2860=CARTESIAN_POINT('Ctrl Pts',(-0.880080083275105,-23.6679643912945,
-0.0391832787017875));
#2861=CARTESIAN_POINT('Ctrl Pts',(0.280613059838117,-23.5558755121778,0.0754000546315256));
#2862=CARTESIAN_POINT('Ctrl Pts',(0.876249675472422,-23.6449624877681,0.132691721298213));
#2863=CARTESIAN_POINT('Ctrl Pts',(1.95910840913653,-24.0958987456423,0.247275054631525));
#2864=CARTESIAN_POINT('Ctrl Pts',(2.44527417877255,-24.4573661122303,0.304566721298234));
#2865=CARTESIAN_POINT('Ctrl Pts',(3.19208164797187,-25.370850975575,0.419150054631504));
#2866=CARTESIAN_POINT('Ctrl Pts',(3.45196757401249,-25.9220285865551,0.476441721298107));
#2867=CARTESIAN_POINT('Ctrl Pts',(3.68132649800696,-27.086466352565,0.591025054631631));
#2868=CARTESIAN_POINT('Ctrl Pts',(3.65052759374337,-27.6986230455641,0.648316721298202));
#2869=CARTESIAN_POINT('Ctrl Pts',(3.30188719744899,-28.840293280662,0.762900054631536));
#2870=CARTESIAN_POINT('Ctrl Pts',(2.98432799528007,-29.3686991601337,0.820191721298178));
#2871=CARTESIAN_POINT('Ctrl Pts',(2.13379161736112,-30.2160978476585,0.93477505463156));
#2872=CARTESIAN_POINT('Ctrl Pts',(1.60159021920541,-30.5342421833904,0.992066721298095));
#2873=CARTESIAN_POINT('Ctrl Pts',(0.445414365419992,-30.8826457776052,1.10665005463164));
#2874=CARTESIAN_POINT('Ctrl Pts',(-0.177469626200369,-30.9125205315103,
1.16394172129828));
#2875=CARTESIAN_POINT('Ctrl Pts',(-1.36813545072923,-30.673420224889,1.27852505463146));
#2876=CARTESIAN_POINT('Ctrl Pts',(-1.93476784632414,-30.4046213916764,1.33581672129817));
#2877=CARTESIAN_POINT('Ctrl Pts',(-2.87746876656431,-29.6280965564544,1.45040005463156));
#2878=CARTESIAN_POINT('Ctrl Pts',(-3.25260154395457,-29.1210720052738,1.50769172129813));
#2879=CARTESIAN_POINT('Ctrl Pts',(-3.72058112180538,-27.9854716656758,1.62227505463161));
#2880=CARTESIAN_POINT('Ctrl Pts',(-3.81293080022416,-27.3579617136213,1.67956672129819));
#2881=CARTESIAN_POINT('Ctrl Pts',(-3.68965672710377,-26.1289746995567,1.79415005463154));
#2882=CARTESIAN_POINT('Ctrl Pts',(-3.47409763241299,-25.5286785378583,1.85144172129826));
#2883=CARTESIAN_POINT('Ctrl Pts',(-2.7822022944777,-24.4971775102941,1.96602505463148));
#2884=CARTESIAN_POINT('Ctrl Pts',(-2.30648341649853,-24.0669891197329,2.02331672129817));
#2885=CARTESIAN_POINT('Ctrl Pts',(-1.20394931882625,-23.4801881039745,2.13790005463157));
#2886=CARTESIAN_POINT('Ctrl Pts',(-0.578163556381753,-23.3241840203502,
2.19519172129821));
#2887=CARTESIAN_POINT('Ctrl Pts',(0.677706928819897,-23.3264027024885,2.30977505463153));
#2888=CARTESIAN_POINT('Ctrl Pts',(1.30659028017156,-23.4846768712254,2.36706672129824));
#2889=CARTESIAN_POINT('Ctrl Pts',(2.4192139548323,-24.0819023526662,2.4816500546315));
#2890=CARTESIAN_POINT('Ctrl Pts',(2.90186470540991,-24.520329561822,2.53894172129796));
#2891=CARTESIAN_POINT('Ctrl Pts',(3.60541788369249,-25.5772648251282,2.65352505463178));
#2892=CARTESIAN_POINT('Ctrl Pts',(3.82560278426285,-26.1947915469424,2.71081672129833));
#2893=CARTESIAN_POINT('Ctrl Pts',(3.94852237831892,-27.4654507839756,2.82540005463141));
#2894=CARTESIAN_POINT('Ctrl Pts',(3.85108621864684,-28.1173730265607,2.88269172129792));
#2895=CARTESIAN_POINT('Ctrl Pts',(3.35786414074355,-29.3023187604958,2.99727505463182));
#2896=CARTESIAN_POINT('Ctrl Pts',(2.96250059030193,-29.8341882432863,3.05456672129825));
#2897=CARTESIAN_POINT('Ctrl Pts',(1.96359948429421,-30.6510950112551,3.16915005463148));
#2898=CARTESIAN_POINT('Ctrl Pts',(1.36098352674217,-30.93530946333,3.22644172129821));
#2899=CARTESIAN_POINT('Ctrl Pts',(0.0881707793306293,-31.186225511463,3.34102505463152));
#2900=CARTESIAN_POINT('Ctrl Pts',(-0.580818873102875,-31.1526345829163,
3.39831672129799));
#2901=CARTESIAN_POINT('Ctrl Pts',(-1.82822926680315,-30.7719182602131,3.51290005463175));
#2902=CARTESIAN_POINT('Ctrl Pts',(-2.40544119057821,-30.4251058408366,3.57019172129822));
#2903=CARTESIAN_POINT('Ctrl Pts',(-3.33097388542638,-29.4964354556262,3.68477505463152));
#2904=CARTESIAN_POINT('Ctrl Pts',(-3.67837143832636,-28.9154280131467,3.74206672129809));
#2905=CARTESIAN_POINT('Ctrl Pts',(-4.05885095899697,-27.6535120007677,3.85665005463164));
#2906=CARTESIAN_POINT('Ctrl Pts',(-4.09151773713705,-26.9737950497155,3.91394172129795));
#2907=CARTESIAN_POINT('Ctrl Pts',(-3.83086030642645,-25.6747542437711,4.02852505463178));
#2908=CARTESIAN_POINT('Ctrl Pts',(-3.53773294713309,-25.0566835016172,4.08581672129817));
#2909=CARTESIAN_POINT('Ctrl Pts',(-2.69110881318515,-24.0285663387021,4.20040005463157));
#2910=CARTESIAN_POINT('Ctrl Pts',(-2.13838054880758,-23.6195373774773,4.25769172129816));
#2911=CARTESIAN_POINT('Ctrl Pts',(-0.900693208979911,-23.1092719795712,
4.37227505463158));
#2912=CARTESIAN_POINT('Ctrl Pts',(-0.216897629946524,-23.0085731171096,
4.42956672129816));
#2913=CARTESIAN_POINT('Ctrl Pts',(1.12205547802317,-23.1426779051177,4.54415005463158));
#2914=CARTESIAN_POINT('Ctrl Pts',(1.77592690914455,-23.377406537751,4.60144172129823));
#2915=CARTESIAN_POINT('Ctrl Pts',(2.89930380962407,-24.1306913712844,4.71602505463151));
#2916=CARTESIAN_POINT('Ctrl Pts',(3.36770491189876,-24.6485714795865,4.77331672129828));
#2917=CARTESIAN_POINT('Ctrl Pts',(4.00659440576528,-25.8485562655112,4.88790005463146));
#2918=CARTESIAN_POINT('Ctrl Pts',(4.17642442602432,-26.5295382611225,4.94519172129826));
#2919=CARTESIAN_POINT('Ctrl Pts',(4.17420574390762,-27.8959069191205,5.05977505463148));
#2920=CARTESIAN_POINT('Ctrl Pts',(4.00210563848955,-28.579986503623,5.117066721298));
#2921=CARTESIAN_POINT('Ctrl Pts',(3.35279167899019,-29.790060866568,5.23165005463174));
#2922=CARTESIAN_POINT('Ctrl Pts',(2.87615175807469,-30.3148728474364,5.28894172129792));
#2923=CARTESIAN_POINT('Ctrl Pts',(1.72734062189585,-31.0798155213496,5.40352505463181));
#2924=CARTESIAN_POINT('Ctrl Pts',(1.0562386306333,-31.319169959825,5.46081672129828));
#2925=CARTESIAN_POINT('Ctrl Pts',(-0.324386700297064,-31.4529202688109,
5.57540005463146));
#2926=CARTESIAN_POINT('Ctrl Pts',(-1.03259456986735,-31.3471349250583,5.63269172129805));
#2927=CARTESIAN_POINT('Ctrl Pts',(-2.3196273040273,-30.8116270271329,5.74727505463168));
#2928=CARTESIAN_POINT('Ctrl Pts',(-2.89720050000837,-30.3823672928139,5.80456672129819));
#2929=CARTESIAN_POINT('Ctrl Pts',(-3.78420656672073,-29.2980499441837,5.91915005463154));
#2930=CARTESIAN_POINT('Ctrl Pts',(-4.0927495448434,-28.643995640032,5.97644172129792));
#2931=CARTESIAN_POINT('Ctrl Pts',(-4.36522271711388,-27.2628079112337,6.09102505463182));
#2932=CARTESIAN_POINT('Ctrl Pts',(-4.32883976428306,-26.5369852993421,6.14831672129839));
#2933=CARTESIAN_POINT('Ctrl Pts',(-3.91604751517395,-25.183834747072,6.26290005463135));
#2934=CARTESIAN_POINT('Ctrl Pts',(-3.5399818785771,-24.5578167789666,6.32019172129842));
#2935=CARTESIAN_POINT('Ctrl Pts',(-2.53317748609787,-23.5541500768163,6.43477505463132));
#2936=CARTESIAN_POINT('Ctrl Pts',(-1.90336399926294,-23.1774993067315,6.49206672129798));
#2937=CARTESIAN_POINT('Ctrl Pts',(-0.535707828330981,-22.7649438596174,
6.60665005463175));
#2938=CARTESIAN_POINT('Ctrl Pts',(0.20084208219242,-22.7294850572333,6.66394172129835));
#2939=CARTESIAN_POINT('Ctrl Pts',(1.6082578695142,-23.011699612039,6.77852505463139));
#2940=CARTESIAN_POINT('Ctrl Pts',(2.27776695825421,-23.3291554974211,6.8358167212985));
#2941=CARTESIAN_POINT('Ctrl Pts',(3.39130036382811,-24.2458789300732,6.95040005463124));
#2942=CARTESIAN_POINT('Ctrl Pts',(3.83422550889456,-24.8443109076698,7.00769172129807));
#2943=CARTESIAN_POINT('Ctrl Pts',(4.38677672685788,-26.1840852477049,7.12227505463167));
#2944=CARTESIAN_POINT('Ctrl Pts',(4.49582477336048,-26.9241664537426,7.17956672129841));
#2945=CARTESIAN_POINT('Ctrl Pts',(4.35088927046636,-28.3730856555887,7.29415005463133));
#2946=CARTESIAN_POINT('Ctrl Pts',(4.09699109987682,-29.0805323561617,7.35144172129841));
#2947=CARTESIAN_POINT('Ctrl Pts',(3.2823167707711,-30.295785129528,7.46602505463132));
#2948=CARTESIAN_POINT('Ctrl Pts',(2.72227543212691,-30.8023989435457,7.52331672129839));
#2949=CARTESIAN_POINT('Ctrl Pts',(1.42483995796224,-31.4933769154898,7.63790005463135));
#2950=CARTESIAN_POINT('Ctrl Pts',(0.688661729169898,-31.6770328723976,7.69519172129708));
#2951=CARTESIAN_POINT('Ctrl Pts',(-0.788205101608382,-31.674814190305,7.80977505463266));
#2952=CARTESIAN_POINT('Ctrl Pts',(-1.52748091929412,-31.4888881482022,7.8670667212985));
#2953=CARTESIAN_POINT('Ctrl Pts',(-2.8350059704747,-30.7874857106489,7.98165005463124));
#2954=CARTESIAN_POINT('Ctrl Pts',(-3.40197918167132,-30.2726330779668,8.03894172129796));
#2955=CARTESIAN_POINT('Ctrl Pts',(-4.22831135118872,-29.0319460689245,8.15352505463178));
#2956=CARTESIAN_POINT('Ctrl Pts',(-4.48683532758525,-28.3072688081897,8.21081672129796));
#2957=CARTESIAN_POINT('Ctrl Pts',(-4.63141635149551,-26.8166773834008,8.32540005463178));
#2958=CARTESIAN_POINT('Ctrl Pts',(-4.51728182365347,-26.0521838868123,8.38269172129824));
#2959=CARTESIAN_POINT('Ctrl Pts',(-3.93948810572916,-24.6630641524548,8.4972750546315));
#2960=CARTESIAN_POINT('Ctrl Pts',(-3.47633218752115,-24.0397872432635,8.55456672129809));
#2961=CARTESIAN_POINT('Ctrl Pts',(-2.30659859626835,-23.0826818778197,8.66915005463165));
#2962=CARTESIAN_POINT('Ctrl Pts',(-1.60110594549963,-22.7498103736324,8.72644172129807));
#2963=CARTESIAN_POINT('Ctrl Pts',(-0.111543235349543,-22.455780077246,8.84102505463166));
#2964=CARTESIAN_POINT('Ctrl Pts',(0.671112336026933,-22.4949550543515,8.89831672129782));
#2965=CARTESIAN_POINT('Ctrl Pts',(2.13000304684827,-22.9398232298639,9.01290005463192));
#2966=CARTESIAN_POINT('Ctrl Pts',(2.80482705930729,-23.3451420836895,9.07019172129816));
#2967=CARTESIAN_POINT('Ctrl Pts',(3.88662776873158,-24.4300804834233,9.18477505463157));
#2968=CARTESIAN_POINT('Ctrl Pts',(4.292531756023,-25.1087000146355,9.24206672129765));
#2969=CARTESIAN_POINT('Ctrl Pts',(4.73716312956515,-26.582096344091,9.35665005463209));
#2970=CARTESIAN_POINT('Ctrl Pts',(4.77541395619357,-27.3754792141155,9.4139417212973));
#2971=CARTESIAN_POINT('Ctrl Pts',(4.47164227730762,-28.8912699827844,9.52852505463244));
#2972=CARTESIAN_POINT('Ctrl Pts',(4.12985786582675,-29.6122174181468,9.58581672129757));
#2973=CARTESIAN_POINT('Ctrl Pts',(3.14303513447574,-30.8111670663372,9.70040005463217));
#2974=CARTESIAN_POINT('Ctrl Pts',(2.49889944364267,-31.2879883952817,9.7576917212976));
#2975=CARTESIAN_POINT('Ctrl Pts',(1.05703810342987,-31.8828254332717,9.87227505463214));
#2976=CARTESIAN_POINT('Ctrl Pts',(0.260671270356948,-32.0002226638335,9.92956672129819));
#2977=CARTESIAN_POINT('Ctrl Pts',(-1.29821402533356,-31.8444564460475,10.0441500546315));
#2978=CARTESIAN_POINT('Ctrl Pts',(-2.05923599538643,-31.5713887375034,10.1014417212983));
#2979=CARTESIAN_POINT('Ctrl Pts',(-3.3663646416149,-30.6953249128279,10.2160250546314));
#2980=CARTESIAN_POINT('Ctrl Pts',(-3.91119116738902,-30.0931223438177,10.2733167212985));
#2981=CARTESIAN_POINT('Ctrl Pts',(-4.65425761740862,-28.6982361814583,10.3879000546312));
#2982=CARTESIAN_POINT('Ctrl Pts',(-4.85173951078678,-27.9068617309244,10.4451917212967));
#2983=CARTESIAN_POINT('Ctrl Pts',(-4.85063016993195,-27.113179217683,10.5024833879649));
#2984=CARTESIAN_POINT('Ctrl Pts',(-4.49992140627864,-27.1253399452581,-0.498733174261208));
#2985=CARTESIAN_POINT('Ctrl Pts',(-4.50080185993612,-26.3890420150452,-0.441441507594522));
#2986=CARTESIAN_POINT('Ctrl Pts',(-4.31739811102725,-25.6514017289714,-0.384149840927902));
#2987=CARTESIAN_POINT('Ctrl Pts',(-3.62151869566008,-24.3457674036837,-0.269566507594513));
#2988=CARTESIAN_POINT('Ctrl Pts',(-3.10966150316856,-23.7790475859312,-0.212274840927868));
#2989=CARTESIAN_POINT('Ctrl Pts',(-1.87473664682874,-22.9517793531317,-0.0976915075945471));
#2990=CARTESIAN_POINT('Ctrl Pts',(-1.15282057736006,-22.6920668090806,-0.0403998409278641));
#2991=CARTESIAN_POINT('Ctrl Pts',(0.333130339632276,-22.543943991072,0.074183492405449));
#2992=CARTESIAN_POINT('Ctrl Pts',(1.09574896981128,-22.6557286792713,0.131475159072136));
#2993=CARTESIAN_POINT('Ctrl Pts',(2.48244573188416,-23.2282112934409,0.246058492405449));
#2994=CARTESIAN_POINT('Ctrl Pts',(3.10517686323593,-23.6884110321826,0.303350159072158));
#2995=CARTESIAN_POINT('Ctrl Pts',(4.06264899488962,-24.8523184668817,0.417933492405427));
#2996=CARTESIAN_POINT('Ctrl Pts',(4.39643269933883,-25.5549467222002,0.475225159072031));
#2997=CARTESIAN_POINT('Ctrl Pts',(4.69353288583996,-27.0395441134278,0.589808492405554));
#2998=CARTESIAN_POINT('Ctrl Pts',(4.65651266421214,-27.8201035217474,0.647100159072126));
#2999=CARTESIAN_POINT('Ctrl Pts',(4.21669252519888,-29.2760623484253,0.761683492405459));
#3000=CARTESIAN_POINT('Ctrl Pts',(3.81426212049019,-29.9500534547892,0.818975159072102));
#3001=CARTESIAN_POINT('Ctrl Pts',(2.735157772082,-31.0316481012048,0.933558492405483));
#3002=CARTESIAN_POINT('Ctrl Pts',(2.05947825480693,-31.4381791363691,0.990850159072061));
#3003=CARTESIAN_POINT('Ctrl Pts',(0.591324236677636,-31.8853789313282,1.10543349240552));
#3004=CARTESIAN_POINT('Ctrl Pts',(-0.199761360833674,-31.9255686777873,
1.1627251590722));
#3005=CARTESIAN_POINT('Ctrl Pts',(-1.71213956917068,-31.6265333528055,1.27730849240538));
#3006=CARTESIAN_POINT('Ctrl Pts',(-2.43197499151047,-31.2875418427295,1.3346001590721));
#3007=CARTESIAN_POINT('Ctrl Pts',(-3.63014773197565,-30.3065048723984,1.44918349240549));
#3008=CARTESIAN_POINT('Ctrl Pts',(-4.10730491757991,-29.66535650003,1.50647515907205));
#3009=CARTESIAN_POINT('Ctrl Pts',(-4.70418417300477,-28.2289639772332,1.62105849240553));
#3010=CARTESIAN_POINT('Ctrl Pts',(-4.8232858148679,-27.4350734021293,1.67835015907212));
#3011=CARTESIAN_POINT('Ctrl Pts',(-4.67189865474462,-25.8800484781485,1.79293349240547));
#3012=CARTESIAN_POINT('Ctrl Pts',(-4.40150140270865,-25.1204069187536,1.85022515907218));
#3013=CARTESIAN_POINT('Ctrl Pts',(-3.53111932870988,-23.8146185429076,1.9648084924054));
#3014=CARTESIAN_POINT('Ctrl Pts',(-2.93192261318194,-23.2697505861832,2.022100159072));
#3015=CARTESIAN_POINT('Ctrl Pts',(-1.54267910662356,-22.5251877903681,2.13668349240558));
#3016=CARTESIAN_POINT('Ctrl Pts',(-0.753936040316516,-22.3262524084538,
2.19397515907222));
#3017=CARTESIAN_POINT('Ctrl Pts',(0.829157957605105,-22.3244915018276,2.30855849240537));
#3018=CARTESIAN_POINT('Ctrl Pts',(1.62199449431653,-22.5217211869735,2.36585015907225));
#3019=CARTESIAN_POINT('Ctrl Pts',(3.02507950821547,-23.2696890805772,2.48043349240533));
#3020=CARTESIAN_POINT('Ctrl Pts',(3.63396055598865,-23.8197589845765,2.53772515907179));
#3021=CARTESIAN_POINT('Ctrl Pts',(4.52261828463197,-25.1465597141148,2.65230849240579));
#3022=CARTESIAN_POINT('Ctrl Pts',(4.80150036645811,-25.9220510526903,2.70960015907225));
#3023=CARTESIAN_POINT('Ctrl Pts',(4.96045389944342,-27.5179680639369,2.82418349240533));
#3024=CARTESIAN_POINT('Ctrl Pts',(4.84032002720497,-28.3368723207458,2.88147515907176));
#3025=CARTESIAN_POINT('Ctrl Pts',(4.22555159288363,-29.8256560833971,2.99605849240583));
#3026=CARTESIAN_POINT('Ctrl Pts',(3.73145567047586,-30.4940909276437,3.05335015907218));
#3027=CARTESIAN_POINT('Ctrl Pts',(2.48213199286114,-31.5216623582789,3.16793349240541));
#3028=CARTESIAN_POINT('Ctrl Pts',(1.7280653912543,-31.8797745886219,3.22522515907214));
#3029=CARTESIAN_POINT('Ctrl Pts',(0.135093018310607,-32.1984318993305,3.33980849240545));
#3030=CARTESIAN_POINT('Ctrl Pts',(-0.702299349132642,-32.1586196534296,
3.39710015907191));
#3031=CARTESIAN_POINT('Ctrl Pts',(-2.26399833471994,-31.6867235879184,3.51168349240567));
#3032=CARTESIAN_POINT('Ctrl Pts',(-2.98679548512054,-31.2550399661564,3.56897515907214));
#3033=CARTESIAN_POINT('Ctrl Pts',(-4.14652413908592,-30.0978016102373,3.68355849240545));
#3034=CARTESIAN_POINT('Ctrl Pts',(-4.58230839125774,-29.3733160488965,3.74085015907202));
#3035=CARTESIAN_POINT('Ctrl Pts',(-5.06158411276736,-27.799421871877,3.85543349240557));
#3036=CARTESIAN_POINT('Ctrl Pts',(-5.10456588344323,-26.9515033152352,3.91272515907188));
#3037=CARTESIAN_POINT('Ctrl Pts',(-4.78397343431367,-25.3307501251766,4.02730849240571));
#3038=CARTESIAN_POINT('Ctrl Pts',(-4.42065339828102,-24.5594763565493,4.08460015907228));
#3039=CARTESIAN_POINT('Ctrl Pts',(-3.36951712903428,-23.2758873731723,4.19918349240531));
#3040=CARTESIAN_POINT('Ctrl Pts',(-2.68266504370096,-22.7648340039114,4.25647515907209));
#3041=CARTESIAN_POINT('Ctrl Pts',(-1.14418552040014,-22.1256689283123,4.3710584924055));
#3042=CARTESIAN_POINT('Ctrl Pts',(-0.2940093186021,-21.9982181024529,4.42835015907226));
#3043=CARTESIAN_POINT('Ctrl Pts',(1.370981699579,-22.1604359774898,4.54293349240532));
#3044=CARTESIAN_POINT('Ctrl Pts',(2.18419852812648,-22.4500027673754,4.60022515907215));
#3045=CARTESIAN_POINT('Ctrl Pts',(3.58186277713337,-23.3817743371321,4.71480849240544));
#3046=CARTESIAN_POINT('Ctrl Pts',(4.16494344537974,-24.0231322827754,4.77210015907202));
#3047=CARTESIAN_POINT('Ctrl Pts',(4.96159471944044,-25.5098264778416,4.88668349240556));
#3048=CARTESIAN_POINT('Ctrl Pts',(5.17435603791885,-26.3537657770459,4.94397515907237));
#3049=CARTESIAN_POINT('Ctrl Pts',(5.17611694457037,-28.0473579480475,5.05855849240522));
#3050=CARTESIAN_POINT('Ctrl Pts',(4.96506132280656,-28.8953907176428,5.11585015907192));
#3051=CARTESIAN_POINT('Ctrl Pts',(4.16500495101401,-30.3959264200764,5.23043349240566));
#3052=CARTESIAN_POINT('Ctrl Pts',(3.57672233543479,-31.0469686979372,5.28772515907185));
#3053=CARTESIAN_POINT('Ctrl Pts',(2.15804573279459,-31.997015922367,5.40230849240574));
#3054=CARTESIAN_POINT('Ctrl Pts',(1.32897912502245,-32.2950675420036,5.45960015907202));
#3055=CARTESIAN_POINT('Ctrl Pts',(-0.376903980395488,-32.4648517899521,
5.57418349240557));
#3056=CARTESIAN_POINT('Ctrl Pts',(-1.25209386392467,-32.3363687336658,5.63147515907217));
#3057=CARTESIAN_POINT('Ctrl Pts',(-2.84296462705654,-31.6793144792236,5.74605849240542));
#3058=CARTESIAN_POINT('Ctrl Pts',(-3.55710318428054,-31.1513223730886,5.80335015907193));
#3059=CARTESIAN_POINT('Ctrl Pts',(-4.65477391382974,-29.8165824526497,5.91793349240566));
#3060=CARTESIAN_POINT('Ctrl Pts',(-5.03721467010861,-29.0110775046754,5.97522515907185));
#3061=CARTESIAN_POINT('Ctrl Pts',(-5.37742910500803,-27.3097301500823,6.08980849240574));
#3062=CARTESIAN_POINT('Ctrl Pts',(-5.334824834833,-26.4155048234392,6.1471001590725));
#3063=CARTESIAN_POINT('Ctrl Pts',(-4.83085284284264,-24.7480656790283,6.26168349240508));
#3064=CARTESIAN_POINT('Ctrl Pts',(-4.36991600398824,-23.9764624845173,6.31897515907215));
#3065=CARTESIAN_POINT('Ctrl Pts',(-3.13454364061771,-22.7385998230638,6.43355849240543));
#3066=CARTESIAN_POINT('Ctrl Pts',(-2.36125203513461,-22.2735623538381,6.4908501590721));
#3067=CARTESIAN_POINT('Ctrl Pts',(-0.681617699318414,-21.762210705809,6.60543349240548));
#3068=CARTESIAN_POINT('Ctrl Pts',(0.223133816549338,-21.716436910903,6.66272515907227));
#3069=CARTESIAN_POINT('Ctrl Pts',(1.95226198823211,-22.0585864841759,6.77730849240531));
#3070=CARTESIAN_POINT('Ctrl Pts',(2.77497410322413,-22.4462350461933,6.83460015907242));
#3071=CARTESIAN_POINT('Ctrl Pts',(4.14397932945591,-23.5674706143039,6.94918349240517));
#3072=CARTESIAN_POINT('Ctrl Pts',(4.68892888241214,-24.3000264126609,7.006475159072));
#3073=CARTESIAN_POINT('Ctrl Pts',(5.37037977816506,-25.9405929364001,7.12105849240559));
#3074=CARTESIAN_POINT('Ctrl Pts',(5.50617978802718,-26.847054764966,7.17835015907233));
#3075=CARTESIAN_POINT('Ctrl Pts',(5.33313119808424,-28.6220118772656,7.29293349240526));
#3076=CARTESIAN_POINT('Ctrl Pts',(5.02439487031729,-29.4888039750442,7.35022515907234));
#3077=CARTESIAN_POINT('Ctrl Pts',(4.03123380485844,-30.9783440971367,7.46480849240525));
#3078=CARTESIAN_POINT('Ctrl Pts',(3.34771462904399,-31.5996374769677,7.52210015907212));
#3079=CARTESIAN_POINT('Ctrl Pts',(1.76356974552581,-32.448377229224,7.63668349240547));
#3080=CARTESIAN_POINT('Ctrl Pts',(0.864434213366158,-32.6749644842892,7.6939751590712));
#3081=CARTESIAN_POINT('Ctrl Pts',(-0.939656130655156,-32.6767253909707,
7.80855849240638));
#3082=CARTESIAN_POINT('Ctrl Pts',(-1.84288513321169,-32.4518438325729,7.86585015907242));
#3083=CARTESIAN_POINT('Ctrl Pts',(-3.44087152408535,-31.5996989826189,7.98043349240516));
#3084=CARTESIAN_POINT('Ctrl Pts',(-4.13407503210608,-30.9732036554222,8.03772515907188));
#3085=CARTESIAN_POINT('Ctrl Pts',(-5.14551175227223,-29.4626511797278,8.1523084924057));
#3086=CARTESIAN_POINT('Ctrl Pts',(-5.46273290975301,-28.5800093026908,8.20960015907188));
#3087=CARTESIAN_POINT('Ctrl Pts',(-5.64334787264751,-26.7641601031904,8.3241834924057));
#3088=CARTESIAN_POINT('Ctrl Pts',(-5.50651563230342,-25.8326845928579,8.38147515907216));
#3089=CARTESIAN_POINT('Ctrl Pts',(-4.8071755577774,-24.1397268293227,8.49605849240542));
#3090=CARTESIAN_POINT('Ctrl Pts',(-4.24528726788241,-23.3798845590642,8.55335015907201));
#3091=CARTESIAN_POINT('Ctrl Pts',(-2.8251311046479,-22.2121145306378,8.66793349240557));
#3092=CARTESIAN_POINT('Ctrl Pts',(-1.96818781025068,-21.8053452483902,8.72522515907199));
#3093=CARTESIAN_POINT('Ctrl Pts',(-0.158465474090509,-21.4435736893289,
8.83980849240559));
#3094=CARTESIAN_POINT('Ctrl Pts',(0.792592811825796,-21.4889699837715,8.89710015907174));
#3095=CARTESIAN_POINT('Ctrl Pts',(2.56577211499604,-22.0250179022253,9.01168349240585));
#3096=CARTESIAN_POINT('Ctrl Pts',(3.38618135368034,-22.5152079582028,9.06897515907209));
#3097=CARTESIAN_POINT('Ctrl Pts',(4.70217802256045,-23.8287143289791,9.1835584924055));
#3098=CARTESIAN_POINT('Ctrl Pts',(5.19646870888364,-24.6508119786607,9.24085015907157));
#3099=CARTESIAN_POINT('Ctrl Pts',(5.7398962834063,-26.4361864732067,9.35543349240601));
#3100=CARTESIAN_POINT('Ctrl Pts',(5.78846210254197,-27.3977709483694,9.41272515907122));
#3101=CARTESIAN_POINT('Ctrl Pts',(5.42475540515261,-29.2352741016053,9.52730849240636));
#3102=CARTESIAN_POINT('Ctrl Pts',(5.01277831711823,-30.1094245630356,9.58460015907149));
#3103=CARTESIAN_POINT('Ctrl Pts',(3.82144345018127,-31.5638460320461,9.69918349240609));
#3104=CARTESIAN_POINT('Ctrl Pts',(3.04318393874474,-32.142691768759,9.75647515907152));
#3105=CARTESIAN_POINT('Ctrl Pts',(1.30053041464135,-32.8664284846192,9.87105849240607));
#3106=CARTESIAN_POINT('Ctrl Pts',(0.337782959236464,-33.0105776785097,9.92835015907211));
#3107=CARTESIAN_POINT('Ctrl Pts',(-1.54714024711339,-32.8266983736559,10.0429334924055));
#3108=CARTESIAN_POINT('Ctrl Pts',(-2.46750761418241,-32.4987925079987,10.1002251590722));
#3109=CARTESIAN_POINT('Ctrl Pts',(-4.0489236093102,-31.4442419468603,10.2148084924053));
#3110=CARTESIAN_POINT('Ctrl Pts',(-4.7084297007651,-30.7185615408183,10.2721001590725));
#3111=CARTESIAN_POINT('Ctrl Pts',(-5.60925793118873,-29.0369659689382,10.3866834924051));
#3112=CARTESIAN_POINT('Ctrl Pts',(-5.8496711226493,-28.082634217585,10.4439751590706));
#3113=CARTESIAN_POINT('Ctrl Pts',(-5.85055157621059,-27.1253399452577,10.5012668257388));
#3114=CARTESIAN_POINT('Ctrl Pts',(-4.49992531496272,-27.2248831058227,0.496297452001021));
#3115=CARTESIAN_POINT('Ctrl Pts',(-4.5170934804426,-26.4885845360516,0.553589118667707));
#3116=CARTESIAN_POINT('Ctrl Pts',(-4.34996170166829,-25.7468676545126,0.610880785334326));
#3117=CARTESIAN_POINT('Ctrl Pts',(-3.68281064144925,-24.4258762531054,0.725464118667716));
#3118=CARTESIAN_POINT('Ctrl Pts',(-3.18338235197652,-23.8478906453164,0.782755785334401));
#3119=CARTESIAN_POINT('Ctrl Pts',(-1.96655436736188,-22.9935362276632,0.897339118667641));
#3120=CARTESIAN_POINT('Ctrl Pts',(-1.2502889550967,-22.7180291994921,0.954630785334324));
#3121=CARTESIAN_POINT('Ctrl Pts',(0.232470285055687,-22.537487692811,1.06921411866772));
#3122=CARTESIAN_POINT('Ctrl Pts',(0.997550948764801,-22.6326791882398,1.12650578533436));
#3123=CARTESIAN_POINT('Ctrl Pts',(2.39671496721365,-23.1750665254593,1.24108911866768));
#3124=CARTESIAN_POINT('Ctrl Pts',(3.02943939521195,-23.6217929692252,1.29838078533443));
#3125=CARTESIAN_POINT('Ctrl Pts',(4.01209348072769,-24.7650357631989,1.41296411866761));
#3126=CARTESIAN_POINT('Ctrl Pts',(4.36104175327124,-25.4604924406082,1.47025578533422));
#3127=CARTESIAN_POINT('Ctrl Pts',(4.69009168456907,-26.9387359366337,1.58483911866782));
#3128=CARTESIAN_POINT('Ctrl Pts',(4.66982607643029,-27.7201191058137,1.64213078533435));
#3129=CARTESIAN_POINT('Ctrl Pts',(4.26117830221042,-29.18553530264,1.75671411866769));
#3130=CARTESIAN_POINT('Ctrl Pts',(3.87313582923077,-29.8681509713484,1.81400578533433));
#3131=CARTESIAN_POINT('Ctrl Pts',(2.81706487876742,-30.9727808246477,1.92858911866771));
#3132=CARTESIAN_POINT('Ctrl Pts',(2.15000879388831,-31.3937004688027,1.98588078533433));
#3133=CARTESIAN_POINT('Ctrl Pts',(0.691309697839529,-31.8720733711749,2.10046411866771));
#3134=CARTESIAN_POINT('Ctrl Pts',(-0.0989534545953723,-31.9290177957557,
2.15775578533426));
#3135=CARTESIAN_POINT('Ctrl Pts',(-1.61768806720869,-31.6619317164947,2.27233911866778));
#3136=CARTESIAN_POINT('Ctrl Pts',(-2.34469625833983,-31.3381042112553,2.32963078533433));
#3137=CARTESIAN_POINT('Ctrl Pts',(-3.56353561707773,-30.3822475718731,2.44421411866772));
#3138=CARTESIAN_POINT('Ctrl Pts',(-4.05416688239932,-29.7510914380183,2.50150578533428));
#3139=CARTESIAN_POINT('Ctrl Pts',(-4.68114239378513,-28.3271638081165,2.61608911866776));
#3140=CARTESIAN_POINT('Ctrl Pts',(-4.81683742169616,-27.5357339634246,2.67338078533435));
#3141=CARTESIAN_POINT('Ctrl Pts',(-4.69786869951757,-25.9775148166942,2.7879641186677));
#3142=CARTESIAN_POINT('Ctrl Pts',(-4.44326548776946,-25.212221359738,2.84525578533441));
#3143=CARTESIAN_POINT('Ctrl Pts',(-3.59996817737392,-23.8883339850702,2.95983911866763));
#3144=CARTESIAN_POINT('Ctrl Pts',(-3.01203627575868,-23.3310362406515,3.01713078533432));
#3145=CARTESIAN_POINT('Ctrl Pts',(-1.6381475891734,-22.5577438837235,3.13171411866773));
#3146=CARTESIAN_POINT('Ctrl Pts',(-0.853479840438057,-22.3425362112162,
3.18900578533436));
#3147=CARTESIAN_POINT('Ctrl Pts',(0.72961543659743,-22.3081998816971,3.30358911866768));
#3148=CARTESIAN_POINT('Ctrl Pts',(1.52652856876947,-22.4891575963454,3.3608807853344));
#3149=CARTESIAN_POINT('Ctrl Pts',(2.94497065879964,-23.2083971347751,3.47546411866765));
#3150=CARTESIAN_POINT('Ctrl Pts',(3.56511749658876,-23.7460381357776,3.5327557853342));
#3151=CARTESIAN_POINT('Ctrl Pts',(4.48086141011516,-25.0547419935726,3.64733911866784));
#3152=CARTESIAN_POINT('Ctrl Pts',(4.77553797602982,-25.8245826749535,3.70463078533439));
#3153=CARTESIAN_POINT('Ctrl Pts',(4.96691019772129,-27.4173080093605,3.81921411866765));
#3154=CARTESIAN_POINT('Ctrl Pts',(4.86336951822156,-28.2386742996913,3.87650578533407));
#3155=CARTESIAN_POINT('Ctrl Pts',(4.27869636088015,-29.7399253187347,3.99108911866797));
#3156=CARTESIAN_POINT('Ctrl Pts',(3.79807373342137,-30.4183534596066,4.0483807853344));
#3157=CARTESIAN_POINT('Ctrl Pts',(2.56941469655591,-31.4711068441301,4.16296411866764));
#3158=CARTESIAN_POINT('Ctrl Pts',(1.82251967284502,-31.8443836425387,4.22025578533436));
#3159=CARTESIAN_POINT('Ctrl Pts',(0.23590119510592,-32.1949906980752,4.33483911866768));
#3160=CARTESIAN_POINT('Ctrl Pts',(-0.602314933192407,-32.1719330656341,
4.39213078533414));
#3161=CARTESIAN_POINT('Ctrl Pts',(-2.17347128894129,-31.7312093649436,4.5067141186679));
#3162=CARTESIAN_POINT('Ctrl Pts',(-2.9048930016682,-31.313913674884,4.56400578533437));
#3163=CARTESIAN_POINT('Ctrl Pts',(-4.08765686254034,-30.1797087169358,4.67858911866767));
#3164=CARTESIAN_POINT('Ctrl Pts',(-4.53782972367693,-29.4638465879738,4.73588078533424));
#3165=CARTESIAN_POINT('Ctrl Pts',(-5.04827855262831,-27.899407333043,4.8504641186678));
#3166=CARTESIAN_POINT('Ctrl Pts',(-5.10801500139697,-27.0523112214756,4.90775578533411));
#3167=CARTESIAN_POINT('Ctrl Pts',(-4.81937179801766,-25.4252016271365,5.02233911866794));
#3168=CARTESIAN_POINT('Ctrl Pts',(-4.4712157667966,-24.6467550897301,5.07963078533432));
#3169=CARTESIAN_POINT('Ctrl Pts',(-3.44525982851924,-23.3424994880601,5.19421411866772));
#3170=CARTESIAN_POINT('Ctrl Pts',(-2.76839998168555,-22.8179720391072,5.25150578533431));
#3171=CARTESIAN_POINT('Ctrl Pts',(-1.24238535128709,-22.1487107075167,5.36608911866773));
#3172=CARTESIAN_POINT('Ctrl Pts',(-0.394669879900677,-22.0046664956406,
5.42338078533431));
#3173=CARTESIAN_POINT('Ctrl Pts',(1.2735153610365,-22.1344659327008,5.53796411866773));
#3174=CARTESIAN_POINT('Ctrl Pts',(2.09238408713078,-22.4082386823275,5.59525578533438));
#3175=CARTESIAN_POINT('Ctrl Pts',(3.50814733498208,-23.3129254884552,5.70983911866766));
#3176=CARTESIAN_POINT('Ctrl Pts',(4.10365779089971,-23.9430186202042,5.76713078533443));
#3177=CARTESIAN_POINT('Ctrl Pts',(4.92903862609668,-25.4143579952863,5.88171411866761));
#3178=CARTESIAN_POINT('Ctrl Pts',(5.15807223514289,-26.2542219769244,5.93900578533441));
#3179=CARTESIAN_POINT('Ctrl Pts',(5.1924085647145,-27.9478154270399,6.05358911866763));
#3180=CARTESIAN_POINT('Ctrl Pts',(4.99762491342332,-28.7999247920913,6.11088078533415));
#3181=CARTESIAN_POINT('Ctrl Pts',(4.22629689682747,-30.315817570665,6.22546411866789));
#3182=CARTESIAN_POINT('Ctrl Pts',(3.65044318422569,-30.978125638526,6.28275578533408));
#3183=CARTESIAN_POINT('Ctrl Pts',(2.24986345334479,-31.9552590478615,6.39733911866797));
#3184=CARTESIAN_POINT('Ctrl Pts',(1.42644750275535,-32.2691051515638,6.45463078533443));
#3185=CARTESIAN_POINT('Ctrl Pts',(-0.276243925815165,-32.4713080882415,
6.56921411866761));
#3186=CARTESIAN_POINT('Ctrl Pts',(-1.15389584286732,-32.3594182246709,6.62650578533421));
#3187=CARTESIAN_POINT('Ctrl Pts',(-2.75723386239692,-31.7324592472316,6.74108911866784));
#3188=CARTESIAN_POINT('Ctrl Pts',(-3.48136571623396,-31.2179404360269,6.79838078533435));
#3189=CARTESIAN_POINT('Ctrl Pts',(-4.60421839969041,-29.9038651563518,6.9129641186677));
#3190=CARTESIAN_POINT('Ctrl Pts',(-5.00182372401274,-29.1055317862615,6.97025578533408));
#3191=CARTESIAN_POINT('Ctrl Pts',(-5.37398790376543,-27.4105383268823,7.08483911866797));
#3192=CARTESIAN_POINT('Ctrl Pts',(-5.34813824702216,-26.5154892393799,7.14213078533454));
#3193=CARTESIAN_POINT('Ctrl Pts',(-4.87533861988318,-24.8385927248065,7.2567141186675));
#3194=CARTESIAN_POINT('Ctrl Pts',(-4.42878971270738,-24.0583649679817,7.31400578533457));
#3195=CARTESIAN_POINT('Ctrl Pts',(-3.21645074732456,-22.7974670995972,7.42858911866747));
#3196=CARTESIAN_POINT('Ctrl Pts',(-2.45178257420817,-22.3180410214301,7.48588078533414));
#3197=CARTESIAN_POINT('Ctrl Pts',(-0.781603160488131,-21.7755162659369,
7.60046411866791));
#3198=CARTESIAN_POINT('Ctrl Pts',(0.122325910305338,-21.7129877929629,7.6577557853345));
#3199=CARTESIAN_POINT('Ctrl Pts',(1.85781048627581,-22.0231881204583,7.77233911866754));
#3200=CARTESIAN_POINT('Ctrl Pts',(2.68769537003688,-22.3956726776898,7.82963078533388));
#3201=CARTESIAN_POINT('Ctrl Pts',(4.07736721457463,-23.4917279148069,7.94421411866817));
#3202=CARTESIAN_POINT('Ctrl Pts',(4.63579084720592,-24.2142914746826,8.00150578533422));
#3203=CARTESIAN_POINT('Ctrl Pts',(5.34733799897106,-25.842393105507,8.11608911866782));
#3204=CARTESIAN_POINT('Ctrl Pts',(5.49973139482918,-26.7463942036693,8.17338078533455));
#3205=CARTESIAN_POINT('Ctrl Pts',(5.35910124288347,-28.5245455387212,8.28796411866749));
#3206=CARTESIAN_POINT('Ctrl Pts',(5.06615895535571,-29.3969895340438,8.34525578533457));
#3207=CARTESIAN_POINT('Ctrl Pts',(4.10008265354488,-30.9046286549901,8.45983911866747));
#3208=CARTESIAN_POINT('Ctrl Pts',(3.42782829160734,-31.5383518224792,8.51713078533533));
#3209=CARTESIAN_POINT('Ctrl Pts',(1.85903822808905,-32.4158211358887,8.63171411866672));
#3210=CARTESIAN_POINT('Ctrl Pts',(0.9639780134877,-32.6586806815057,8.68900578533323));
#3211=CARTESIAN_POINT('Ctrl Pts',(-0.840113609647483,-32.6930170111224,
8.80358911866881));
#3212=CARTESIAN_POINT('Ctrl Pts',(-1.74741920765194,-32.4844074231763,8.86088078533465));
#3213=CARTESIAN_POINT('Ctrl Pts',(-3.3607626746822,-31.6609909284457,8.97546411866739));
#3214=CARTESIAN_POINT('Ctrl Pts',(-4.06523197268589,-31.0469245042064,9.03275578533411));
#3215=CARTESIAN_POINT('Ctrl Pts',(-5.10375487777573,-29.5544689002848,9.14733911866793));
#3216=CARTESIAN_POINT('Ctrl Pts',(-5.43677051929896,-28.6774776804222,9.20463078533411));
#3217=CARTESIAN_POINT('Ctrl Pts',(-5.64980417095116,-26.8648201577722,9.31921411866793));
#3218=CARTESIAN_POINT('Ctrl Pts',(-5.5295651232969,-25.9308826139232,9.37650578533439));
#3219=CARTESIAN_POINT('Ctrl Pts',(-4.86032032579704,-24.2254575939744,9.49108911866765));
#3220=CARTESIAN_POINT('Ctrl Pts',(-4.31190533081157,-23.4556220271188,9.54838078533424));
#3221=CARTESIAN_POINT('Ctrl Pts',(-2.91241380835902,-22.2626700447691,9.6629641186678));
#3222=CARTESIAN_POINT('Ctrl Pts',(-2.06264209183543,-21.8407361944978,9.72025578533422));
#3223=CARTESIAN_POINT('Ctrl Pts',(-0.259273650891808,-21.4470148905597,
9.83483911866782));
#3224=CARTESIAN_POINT('Ctrl Pts',(0.692608395878797,-21.4756565715901,9.89213078533397));
#3225=CARTESIAN_POINT('Ctrl Pts',(2.47524506922415,-21.9805321251769,10.0067141186681));
#3226=CARTESIAN_POINT('Ctrl Pts',(3.30427887021131,-22.4563342494898,10.0640057853343));
#3227=CARTESIAN_POINT('Ctrl Pts',(4.64331074603158,-23.7468072222661,10.1785891186677));
#3228=CARTESIAN_POINT('Ctrl Pts',(5.15199004128089,-24.5602814395911,10.2358807853338));
#3229=CARTESIAN_POINT('Ctrl Pts',(5.7265907232892,-26.336201012033,10.3504641186682));
#3230=CARTESIAN_POINT('Ctrl Pts',(5.79191122047382,-27.2969630421229,10.4077557853326));
#3231=CARTESIAN_POINT('Ctrl Pts',(5.4601537688785,-29.1408225996516,10.5223391186694));
#3232=CARTESIAN_POINT('Ctrl Pts',(5.06334068561503,-30.0221458298436,10.5796307853337));
#3233=CARTESIAN_POINT('Ctrl Pts',(3.897186149685,-31.4972339171696,10.6942141186683));
#3234=CARTESIAN_POINT('Ctrl Pts',(3.12891887671996,-32.0895537335424,10.7515057853337));
#3235=CARTESIAN_POINT('Ctrl Pts',(1.39873024553766,-32.8433867054356,10.8660891186683));
#3236=CARTESIAN_POINT('Ctrl Pts',(0.438443520536697,-33.0041292853017,10.9233807853343));
#3237=CARTESIAN_POINT('Ctrl Pts',(-1.44967390857254,-32.8526684184651,11.0379641186677));
#3238=CARTESIAN_POINT('Ctrl Pts',(-2.37569317317473,-32.5405565930317,11.0952557853345));
#3239=CARTESIAN_POINT('Ctrl Pts',(-3.97520816717089,-31.5130907955522,11.2098391186676));
#3240=CARTESIAN_POINT('Ctrl Pts',(-4.64714404626587,-30.7986752033783,11.2671307853347));
#3241=CARTESIAN_POINT('Ctrl Pts',(-5.57670183786417,-29.1324344515049,11.3817141186674));
#3242=CARTESIAN_POINT('Ctrl Pts',(-5.83338731961563,-28.1821780177065,11.4390057853329));
#3243=CARTESIAN_POINT('Ctrl Pts',(-5.85055548489467,-27.2248831058223,11.496297452001));
#3244=CARTESIAN_POINT('Ctrl Pts',(-3.50000130290148,-27.2127226059667,0.497516610448255));
#3245=CARTESIAN_POINT('Ctrl Pts',(-3.51517971121378,-26.6400362227171,0.554808277114941));
#3246=CARTESIAN_POINT('Ctrl Pts',(-3.38700359289755,-26.0622729395371,0.612099943781561));
#3247=CARTESIAN_POINT('Ctrl Pts',(-2.87059541238073,-25.0317435939839,0.72668327711495));
#3248=CARTESIAN_POINT('Ctrl Pts',(-2.48281014130459,-24.5799885832371,0.783974943781635));
#3249=CARTESIAN_POINT('Ctrl Pts',(-1.53584837306688,-23.9107391275463,0.898558277114875));
#3250=CARTESIAN_POINT('Ctrl Pts',(-0.977548004253359,-23.6939293925514,
0.955849943781558));
#3251=CARTESIAN_POINT('Ctrl Pts',(0.179952606081418,-23.5494218341822,1.07043327711495));
#3252=CARTESIAN_POINT('Ctrl Pts',(0.778050826506515,-23.6219155146099,1.1277249437816));
#3253=CARTESIAN_POINT('Ctrl Pts',(1.87337605723642,-24.0427561003574,1.24230827711491));
#3254=CARTESIAN_POINT('Ctrl Pts',(2.36953479367315,-24.3907498795612,1.29959994378166));
#3255=CARTESIAN_POINT('Ctrl Pts',(3.14152373336449,-25.2835693957278,1.41418327711485));
#3256=CARTESIAN_POINT('Ctrl Pts',(3.41657407444237,-25.8275750154296,1.47147494378145));
#3257=CARTESIAN_POINT('Ctrl Pts',(3.67788264996072,-26.9856580353439,1.58605827711506));
#3258=CARTESIAN_POINT('Ctrl Pts',(3.66383841906194,-27.5986380524938,1.64334994378159));
#3259=CARTESIAN_POINT('Ctrl Pts',(3.34637070640969,-28.7497648633494,1.75793327711492));
#3260=CARTESIAN_POINT('Ctrl Pts',(3.04319969463925,-29.2867949482463,1.81522494378156));
#3261=CARTESIAN_POINT('Ctrl Pts',(2.21569737033779,-30.1572282923719,1.92980827711495));
#3262=CARTESIAN_POINT('Ctrl Pts',(1.69211980095435,-30.4897610442556,1.98709994378157));
#3263=CARTESIAN_POINT('Ctrl Pts',(0.545399706903326,-30.8693375696566,2.10168327711494));
#3264=CARTESIAN_POINT('Ctrl Pts',(-0.0766613991650282,-30.9159670184662,
2.1589749437815));
#3265=CARTESIAN_POINT('Ctrl Pts',(-1.27368280615195,-30.7088161970159,2.27355827711501));
#3266=CARTESIAN_POINT('Ctrl Pts',(-1.84748758998441,-30.4551815910792,2.33084994378156));
#3267=CARTESIAN_POINT('Ctrl Pts',(-2.81085451659558,-29.7038376853842,2.44543327711495));
#3268=CARTESIAN_POINT('Ctrl Pts',(-3.19946114294195,-29.2068057482841,2.50272494378152));
#3269=CARTESIAN_POINT('Ctrl Pts',(-3.69753671927098,-28.0836711179268,2.61730827711499));
#3270=CARTESIAN_POINT('Ctrl Pts',(-3.806479757265,-27.4586223362847,2.67459994378158));
#3271=CARTESIAN_POINT('Ctrl Pts',(-3.71562427983475,-26.2264419408016,2.78918327711493));
#3272=CARTESIAN_POINT('Ctrl Pts',(-3.51585940949974,-25.6204942820667,2.84647494378164));
#3273=CARTESIAN_POINT('Ctrl Pts',(-2.85104937088523,-24.5708949233056,2.96105827711487));
#3274=CARTESIAN_POINT('Ctrl Pts',(-2.38659565795852,-24.1282770115141,3.01834994378155));
#3275=CARTESIAN_POINT('Ctrl Pts',(-1.29941716743804,-23.5127467708991,3.13293327711496));
#3276=CARTESIAN_POINT('Ctrl Pts',(-0.677707157851868,-23.3404704661548,
3.19022494378159));
#3277=CARTESIAN_POINT('Ctrl Pts',(0.578163753723292,-23.3101136508809,3.30480827711492));
#3278=CARTESIAN_POINT('Ctrl Pts',(1.21112328389688,-23.4521157051967,3.36209994378163));
#3279=CARTESIAN_POINT('Ctrl Pts',(2.33910331776924,-24.020612363763,3.47668327711488));
#3280=CARTESIAN_POINT('Ctrl Pts',(2.83301955876491,-24.4466103465917,3.53397494378134));
#3281=CARTESIAN_POINT('Ctrl Pts',(3.56365851013518,-25.4854479877254,3.64855827711517));
#3282=CARTESIAN_POINT('Ctrl Pts',(3.79963778298962,-26.0973236259647,3.70584994378171));
#3283=CARTESIAN_POINT('Ctrl Pts',(3.95497605633098,-27.3647903302184,3.8204332771148));
#3284=CARTESIAN_POINT('Ctrl Pts',(3.87413319178915,-28.0191741775874,3.87772494378131));
#3285=CARTESIAN_POINT('Ctrl Pts',(3.41100678604432,-29.2165864086031,3.9923082771152));
#3286=CARTESIAN_POINT('Ctrl Pts',(3.02911682295908,-29.7584488581732,4.04959994378164));
#3287=CARTESIAN_POINT('Ctrl Pts',(2.05088106415332,-30.6005370966614,4.16418327711487));
#3288=CARTESIAN_POINT('Ctrl Pts',(1.45543709786498,-30.8999159637434,4.2214749437816));
#3289=CARTESIAN_POINT('Ctrl Pts',(0.188979096554336,-31.1827816634333,4.33605827711491));
#3290=CARTESIAN_POINT('Ctrl Pts',(-0.480833880026034,-31.1659454082194,
4.39334994378137));
#3291=CARTESIAN_POINT('Ctrl Pts',(-1.73770084949707,-30.8164017691893,4.50793327711514));
#3292=CARTESIAN_POINT('Ctrl Pts',(-2.32353697868073,-30.4839775401827,4.5652249437816));
#3293=CARTESIAN_POINT('Ctrl Pts',(-3.2721043301499,-29.5783412086159,4.67980827711491));
#3294=CARTESIAN_POINT('Ctrl Pts',(-3.63389029917657,-29.0059575948908,4.73709994378148));
#3295=CARTESIAN_POINT('Ctrl Pts',(-4.04554275106343,-27.7534973422558,4.85168327711503));
#3296=CARTESIAN_POINT('Ctrl Pts',(-4.09496422407853,-27.0746032767544,4.90897494378134));
#3297=CARTESIAN_POINT('Ctrl Pts',(-3.86625627856773,-25.7692068883448,5.02355827711517));
#3298=CARTESIAN_POINT('Ctrl Pts',(-3.58829314652568,-25.1439637579671,5.08084994378156));
#3299=CARTESIAN_POINT('Ctrl Pts',(-2.76684994212521,-24.0951805886606,5.19543327711495));
#3300=CARTESIAN_POINT('Ctrl Pts',(-2.22411429181341,-23.6726777785058,5.25272494378155));
#3301=CARTESIAN_POINT('Ctrl Pts',(-0.998892661235347,-23.1323163820897,
5.36730827711496));
#3302=CARTESIAN_POINT('Ctrl Pts',(-0.317558252613747,-23.0150241600847,
5.42459994378155));
#3303=CARTESIAN_POINT('Ctrl Pts',(1.02458823678216,-23.1167103523708,5.53918327711497));
#3304=CARTESIAN_POINT('Ctrl Pts',(1.68411116492473,-23.3356447606771,5.59647494378161));
#3305=CARTESIAN_POINT('Ctrl Pts',(2.82558639662397,-24.061844294864,5.7110582771149));
#3306=CARTESIAN_POINT('Ctrl Pts',(3.30641702010581,-24.568459238132,5.76834994378167));
#3307=CARTESIAN_POINT('Ctrl Pts',(3.97403573885252,-25.7530884168939,5.88293327711484));
#3308=CARTESIAN_POINT('Ctrl Pts',(4.16013798020538,-26.4299946596524,5.94022494378164));
#3309=CARTESIAN_POINT('Ctrl Pts',(4.19049479552954,-27.7963637440239,6.05480827711487));
#3310=CARTESIAN_POINT('Ctrl Pts',(4.03466680450649,-28.4845195073438,6.11209994378139));
#3311=CARTESIAN_POINT('Ctrl Pts',(3.41408166790506,-29.7099502295094,6.22668327711512));
#3312=CARTESIAN_POINT('Ctrl Pts',(2.94987097329771,-30.2460277007815,6.28397494378131));
#3313=CARTESIAN_POINT('Ctrl Pts',(1.8191574593059,-31.0380561478021,6.3985582771152));
#3314=CARTESIAN_POINT('Ctrl Pts',(1.15370655160782,-31.2932049585382,6.45584994378166));
#3315=CARTESIAN_POINT('Ctrl Pts',(-0.22372624653663,-31.4593739468365,6.57043327711484));
#3316=CARTESIAN_POINT('Ctrl Pts',(-0.934395720889725,-31.3701818981879,
6.62772494378144));
#3317=CARTESIAN_POINT('Ctrl Pts',(-2.23389495213891,-30.8647696724464,6.74230827711507));
#3318=CARTESIAN_POINT('Ctrl Pts',(-2.82146111488582,-30.4489835254622,6.79959994378158));
#3319=CARTESIAN_POINT('Ctrl Pts',(-3.73364865213651,-29.3853315240515,6.91418327711493));
#3320=CARTESIAN_POINT('Ctrl Pts',(-4.05735604524484,-28.7384492111523,6.97147494378131));
#3321=CARTESIAN_POINT('Ctrl Pts',(-4.36177886909609,-27.3636162284599,7.0860582771152));
#3322=CARTESIAN_POINT('Ctrl Pts',(-4.34215058957306,-26.6369702924209,7.14334994378177));
#3323=CARTESIAN_POINT('Ctrl Pts',(-3.96053102416322,-25.2743631643761,7.25793327711474));
#3324=CARTESIAN_POINT('Ctrl Pts',(-3.59885357791486,-24.6397209908769,7.31522494378181));
#3325=CARTESIAN_POINT('Ctrl Pts',(-2.61508323909598,-23.61301963208,7.4298082771147));
#3326=CARTESIAN_POINT('Ctrl Pts',(-1.9938935810033,-23.2219804458925,7.48709994378137));
#3327=CARTESIAN_POINT('Ctrl Pts',(-0.635693169822906,-22.7782520675398,
7.60168327711514));
#3328=CARTESIAN_POINT('Ctrl Pts',(0.100033855150708,-22.726038570305,7.65897494378174));
#3329=CARTESIAN_POINT('Ctrl Pts',(1.51380522494329,-22.9763036398845,7.77355827711478));
#3330=CARTESIAN_POINT('Ctrl Pts',(2.19048670189786,-23.2785952980398,7.8308499437815));
#3331=CARTESIAN_POINT('Ctrl Pts',(3.32468611387601,-24.1701378011219,7.94543327711501));
#3332=CARTESIAN_POINT('Ctrl Pts',(3.78108510785602,-24.7585771646693,8.00272494378146));
#3333=CARTESIAN_POINT('Ctrl Pts',(4.36373232434941,-26.085885795444,8.11730827711505));
#3334=CARTESIAN_POINT('Ctrl Pts',(4.48937373037522,-26.8235058310766,8.17459994378218));
#3335=CARTESIAN_POINT('Ctrl Pts',(4.37685682322345,-28.2756184143465,8.28918327711433));
#3336=CARTESIAN_POINT('Ctrl Pts',(4.13875287694128,-28.9887166119371,8.3464749437818));
#3337=CARTESIAN_POINT('Ctrl Pts',(3.35116384720094,-30.2220677165326,8.46105827711471));
#3338=CARTESIAN_POINT('Ctrl Pts',(2.80238767357428,-30.741111051742,8.51834994378256));
#3339=CARTESIAN_POINT('Ctrl Pts',(1.52030780658665,-31.4608182485878,8.63293327711395));
#3340=CARTESIAN_POINT('Ctrl Pts',(0.788205330640013,-31.6607464265703,8.69022494378047));
#3341=CARTESIAN_POINT('Ctrl Pts',(-0.688661926511778,-31.6911032419353,
8.80480827711605));
#3342=CARTESIAN_POINT('Ctrl Pts',(-1.43201392300667,-31.5214493142069,8.86209994378189));
#3343=CARTESIAN_POINT('Ctrl Pts',(-2.75489533342443,-30.8487756995759,8.97668327711462));
#3344=CARTESIAN_POINT('Ctrl Pts',(-3.33313403500641,-30.3463522931823,9.03397494378135));
#3345=CARTESIAN_POINT('Ctrl Pts',(-4.18655197765132,-29.123762906342,9.14855827711516));
#3346=CARTESIAN_POINT('Ctrl Pts',(-4.46087032628663,-28.4047367291627,9.20584994378135));
#3347=CARTESIAN_POINT('Ctrl Pts',(-4.63787002953295,-26.9173378371627,9.32043327711516));
#3348=CARTESIAN_POINT('Ctrl Pts',(-4.54032879677263,-26.1503827357956,9.37772494378163));
#3349=CARTESIAN_POINT('Ctrl Pts',(-3.99263075105309,-24.7487965043376,9.49230827711489));
#3350=CARTESIAN_POINT('Ctrl Pts',(-3.54294842016277,-24.1155266283949,9.54959994378147));
#3351=CARTESIAN_POINT('Ctrl Pts',(-2.393880176143,-23.1332397923951,9.66418327711504));
#3352=CARTESIAN_POINT('Ctrl Pts',(-1.69555951661787,-22.7852038732428,9.72147494378146));
#3353=CARTESIAN_POINT('Ctrl Pts',(-0.21235155257781,-22.4592239252521,9.83605827711505));
#3354=CARTESIAN_POINT('Ctrl Pts',(0.571127342942618,-22.4816442290709,9.8933499437812));
#3355=CARTESIAN_POINT('Ctrl Pts',(2.03947462954967,-22.8953397208652,10.0079332771153));
#3356=CARTESIAN_POINT('Ctrl Pts',(2.72292284739241,-23.2862703843579,10.0652249437816));
#3357=CARTESIAN_POINT('Ctrl Pts',(3.82775821347252,-24.3481747304191,10.179808277115));
#3358=CARTESIAN_POINT('Ctrl Pts',(4.24805061685128,-25.0181704328983,10.237099943781));
#3359=CARTESIAN_POINT('Ctrl Pts',(4.72385492165356,-26.4821110025959,10.3516832771155));
#3360=CARTESIAN_POINT('Ctrl Pts',(4.77886044311237,-27.2746709870712,10.4089749437799));
#3361=CARTESIAN_POINT('Ctrl Pts',(4.50703824947158,-28.796817338216,10.5235582771166));
#3362=CARTESIAN_POINT('Ctrl Pts',(4.18041806520056,-29.5249371617849,10.580849943781));
#3363=CARTESIAN_POINT('Ctrl Pts',(3.21877626343458,-30.7445528163907,10.6954332771156));
#3364=CARTESIAN_POINT('Ctrl Pts',(2.58463318663832,-31.2348479942316,10.752724943781));
#3365=CARTESIAN_POINT('Ctrl Pts',(1.15523755569548,-31.8597810307748,10.8673082771155));
#3366=CARTESIAN_POINT('Ctrl Pts',(0.361331893025007,-31.9937716208391,10.9245999437816));
#3367=CARTESIAN_POINT('Ctrl Pts',(-1.20074678409337,-31.8704239988137,11.0391832771149));
#3368=CARTESIAN_POINT('Ctrl Pts',(-1.96742025115454,-31.6131505145616,11.0964749437817));
#3369=CARTESIAN_POINT('Ctrl Pts',(-3.29264722862687,-30.7641719892639,11.2110582771148));
#3370=CARTESIAN_POINT('Ctrl Pts',(-3.84990327557803,-30.1732345852601,11.2683499437819));
#3371=CARTESIAN_POINT('Ctrl Pts',(-4.62169895051392,-28.7937040300877,11.3829332771146));
#3372=CARTESIAN_POINT('Ctrl Pts',(-4.83545306471002,-28.0064053323945,11.4402249437801));
#3373=CARTESIAN_POINT('Ctrl Pts',(-4.85063147283344,-27.2127226059663,11.4975166104483));
#3374=CARTESIAN_POINT('',(-3.5,-27.2127225901214,0.49751661203513));
#3375=CARTESIAN_POINT('',(-3.5,-27.1131792176833,-0.497516612035131));
#3376=CARTESIAN_POINT('Origin',(-3.5,-27.1629509039024,-4.33680868994202E-16));
#3377=CARTESIAN_POINT('',(-4.85063029663924,-27.113179219224,10.5024833878107));
#3378=CARTESIAN_POINT('Ctrl Pts',(-3.5,-27.1131792176833,-0.497516612035131));
#3379=CARTESIAN_POINT('Ctrl Pts',(-3.49889065922935,-26.5404930476192,-0.440224945368445));
#3380=CARTESIAN_POINT('Ctrl Pts',(-3.3544424268553,-25.9668059432703,-0.382933278701826));
#3381=CARTESIAN_POINT('Ctrl Pts',(-3.08187392517324,-25.4592194500916,-0.325641612035131));
#3382=CARTESIAN_POINT('Ctrl Pts',(-2.80930542349117,-24.951632956913,-0.268349945368436));
#3383=CARTESIAN_POINT('Ctrl Pts',(-2.40909092606461,-24.5111434366068,-0.211058278701792));
#3384=CARTESIAN_POINT('Ctrl Pts',(-1.92656123086921,-24.1900615952905,-0.153766612035131));
#3385=CARTESIAN_POINT('Ctrl Pts',(-1.4440315356738,-23.8689797539743,-0.0964749453684703));
#3386=CARTESIAN_POINT('Ctrl Pts',(-0.880080083275106,-23.6679643912945,
-0.0391832787017876));
#3387=CARTESIAN_POINT('Ctrl Pts',(-0.299733511718495,-23.6119199517362,
0.018108387964869));
#3388=CARTESIAN_POINT('Ctrl Pts',(0.280613059838117,-23.5558755121778,0.0754000546315256));
#3389=CARTESIAN_POINT('Ctrl Pts',(0.876249675472422,-23.6449624877681,0.132691721298213));
#3390=CARTESIAN_POINT('Ctrl Pts',(1.41767904230447,-23.8704306167052,0.189983387964869));
#3391=CARTESIAN_POINT('Ctrl Pts',(1.95910840913652,-24.0958987456423,0.247275054631525));
#3392=CARTESIAN_POINT('Ctrl Pts',(2.44527417877255,-24.4573661122303,0.304566721298234));
#3393=CARTESIAN_POINT('Ctrl Pts',(2.81867791337221,-24.9141085439026,0.361858387964869));
#3394=CARTESIAN_POINT('Ctrl Pts',(3.19208164797187,-25.370850975575,0.419150054631504));
#3395=CARTESIAN_POINT('Ctrl Pts',(3.45196757401249,-25.9220285865551,0.476441721298107));
#3396=CARTESIAN_POINT('Ctrl Pts',(3.56664703600973,-26.50424746956,0.533733387964869));
#3397=CARTESIAN_POINT('Ctrl Pts',(3.68132649800696,-27.086466352565,0.591025054631631));
#3398=CARTESIAN_POINT('Ctrl Pts',(3.65052759374337,-27.6986230455641,0.648316721298202));
#3399=CARTESIAN_POINT('Ctrl Pts',(3.47620739559618,-28.2694581631131,0.705608387964869));
#3400=CARTESIAN_POINT('Ctrl Pts',(3.30188719744899,-28.840293280662,0.762900054631535));
#3401=CARTESIAN_POINT('Ctrl Pts',(2.98432799528007,-29.3686991601337,0.820191721298179));
#3402=CARTESIAN_POINT('Ctrl Pts',(2.5590598063206,-29.7923985038961,0.877483387964869));
#3403=CARTESIAN_POINT('Ctrl Pts',(2.13379161736112,-30.2160978476585,0.93477505463156));
#3404=CARTESIAN_POINT('Ctrl Pts',(1.60159021920541,-30.5342421833904,0.992066721298096));
#3405=CARTESIAN_POINT('Ctrl Pts',(1.0235022923127,-30.7084439804978,1.04935838796487));
#3406=CARTESIAN_POINT('Ctrl Pts',(0.445414365419992,-30.8826457776052,1.10665005463164));
#3407=CARTESIAN_POINT('Ctrl Pts',(-0.177469626200368,-30.9125205315103,
1.16394172129828));
#3408=CARTESIAN_POINT('Ctrl Pts',(-0.772802538464799,-30.7929703781997,
1.22123338796487));
#3409=CARTESIAN_POINT('Ctrl Pts',(-1.36813545072923,-30.673420224889,1.27852505463146));
#3410=CARTESIAN_POINT('Ctrl Pts',(-1.93476784632414,-30.4046213916764,1.33581672129817));
#3411=CARTESIAN_POINT('Ctrl Pts',(-2.40611830644423,-30.0163589740654,1.39310838796487));
#3412=CARTESIAN_POINT('Ctrl Pts',(-2.87746876656431,-29.6280965564544,1.45040005463156));
#3413=CARTESIAN_POINT('Ctrl Pts',(-3.25260154395457,-29.1210720052738,1.50769172129813));
#3414=CARTESIAN_POINT('Ctrl Pts',(-3.48659133287997,-28.5532718354748,1.56498338796487));
#3415=CARTESIAN_POINT('Ctrl Pts',(-3.72058112180538,-27.9854716656758,1.62227505463161));
#3416=CARTESIAN_POINT('Ctrl Pts',(-3.81293080022416,-27.3579617136213,1.67956672129819));
#3417=CARTESIAN_POINT('Ctrl Pts',(-3.75129376366397,-26.743468206589,1.73685838796487));
#3418=CARTESIAN_POINT('Ctrl Pts',(-3.68965672710377,-26.1289746995567,1.79415005463154));
#3419=CARTESIAN_POINT('Ctrl Pts',(-3.47409763241299,-25.5286785378583,1.85144172129826));
#3420=CARTESIAN_POINT('Ctrl Pts',(-3.12814996344534,-25.0129280240762,1.90873338796487));
#3421=CARTESIAN_POINT('Ctrl Pts',(-2.7822022944777,-24.4971775102941,1.96602505463148));
#3422=CARTESIAN_POINT('Ctrl Pts',(-2.30648341649854,-24.0669891197329,2.02331672129817));
#3423=CARTESIAN_POINT('Ctrl Pts',(-1.75521636766239,-23.7735886118537,2.08060838796487));
#3424=CARTESIAN_POINT('Ctrl Pts',(-1.20394931882625,-23.4801881039745,2.13790005463157));
#3425=CARTESIAN_POINT('Ctrl Pts',(-0.578163556381755,-23.3241840203502,
2.19519172129821));
#3426=CARTESIAN_POINT('Ctrl Pts',(0.0497716862190717,-23.3252933614194,
2.25248338796487));
#3427=CARTESIAN_POINT('Ctrl Pts',(0.677706928819894,-23.3264027024885,2.30977505463153));
#3428=CARTESIAN_POINT('Ctrl Pts',(1.30659028017156,-23.4846768712254,2.36706672129824));
#3429=CARTESIAN_POINT('Ctrl Pts',(1.86290211750193,-23.7832896119458,2.42435838796487));
#3430=CARTESIAN_POINT('Ctrl Pts',(2.4192139548323,-24.0819023526662,2.4816500546315));
#3431=CARTESIAN_POINT('Ctrl Pts',(2.90186470540991,-24.520329561822,2.53894172129796));
#3432=CARTESIAN_POINT('Ctrl Pts',(3.2536412945512,-25.0487971934751,2.59623338796487));
#3433=CARTESIAN_POINT('Ctrl Pts',(3.6054178836925,-25.5772648251282,2.65352505463178));
#3434=CARTESIAN_POINT('Ctrl Pts',(3.82560278426284,-26.1947915469425,2.71081672129833));
#3435=CARTESIAN_POINT('Ctrl Pts',(3.88706258129088,-26.830121165459,2.76810838796487));
#3436=CARTESIAN_POINT('Ctrl Pts',(3.94852237831892,-27.4654507839756,2.82540005463141));
#3437=CARTESIAN_POINT('Ctrl Pts',(3.85108621864684,-28.1173730265607,2.88269172129792));
#3438=CARTESIAN_POINT('Ctrl Pts',(3.60447517969519,-28.7098458935282,2.93998338796487));
#3439=CARTESIAN_POINT('Ctrl Pts',(3.35786414074354,-29.3023187604958,2.99727505463182));
#3440=CARTESIAN_POINT('Ctrl Pts',(2.96250059030192,-29.8341882432863,3.05456672129825));
#3441=CARTESIAN_POINT('Ctrl Pts',(2.46305003729807,-30.2426416272707,3.11185838796487));
#3442=CARTESIAN_POINT('Ctrl Pts',(1.96359948429421,-30.6510950112551,3.16915005463149));
#3443=CARTESIAN_POINT('Ctrl Pts',(1.36098352674217,-30.93530946333,3.22644172129821));
#3444=CARTESIAN_POINT('Ctrl Pts',(0.7245771530364,-31.0607674873965,3.28373338796487));
#3445=CARTESIAN_POINT('Ctrl Pts',(0.0881707793306251,-31.186225511463,3.34102505463152));
#3446=CARTESIAN_POINT('Ctrl Pts',(-0.580818873102877,-31.1526345829163,
3.39831672129799));
#3447=CARTESIAN_POINT('Ctrl Pts',(-1.20452406995301,-30.9622764215647,3.45560838796487));
#3448=CARTESIAN_POINT('Ctrl Pts',(-1.82822926680315,-30.7719182602131,3.51290005463175));
#3449=CARTESIAN_POINT('Ctrl Pts',(-2.40544119057821,-30.4251058408366,3.57019172129822));
#3450=CARTESIAN_POINT('Ctrl Pts',(-2.86820753800229,-29.9607706482314,3.62748338796487));
#3451=CARTESIAN_POINT('Ctrl Pts',(-3.33097388542638,-29.4964354556262,3.68477505463152));
#3452=CARTESIAN_POINT('Ctrl Pts',(-3.67837143832636,-28.9154280131467,3.74206672129809));
#3453=CARTESIAN_POINT('Ctrl Pts',(-3.86861119866167,-28.2844700069572,3.79935838796487));
#3454=CARTESIAN_POINT('Ctrl Pts',(-4.05885095899697,-27.6535120007677,3.85665005463165));
#3455=CARTESIAN_POINT('Ctrl Pts',(-4.09151773713705,-26.9737950497155,3.91394172129795));
#3456=CARTESIAN_POINT('Ctrl Pts',(-3.96118902178175,-26.3242746467433,3.97123338796487));
#3457=CARTESIAN_POINT('Ctrl Pts',(-3.83086030642645,-25.6747542437711,4.02852505463179));
#3458=CARTESIAN_POINT('Ctrl Pts',(-3.53773294713309,-25.0566835016172,4.08581672129817));
#3459=CARTESIAN_POINT('Ctrl Pts',(-3.11442088015912,-24.5426249201597,4.14310838796487));
#3460=CARTESIAN_POINT('Ctrl Pts',(-2.69110881318516,-24.0285663387021,4.20040005463157));
#3461=CARTESIAN_POINT('Ctrl Pts',(-2.13838054880758,-23.6195373774773,4.25769172129816));
#3462=CARTESIAN_POINT('Ctrl Pts',(-1.51953687889374,-23.3644046785242,4.31498338796487));
#3463=CARTESIAN_POINT('Ctrl Pts',(-0.900693208979914,-23.1092719795712,
4.37227505463158));
#3464=CARTESIAN_POINT('Ctrl Pts',(-0.216897629946521,-23.0085731171096,
4.42956672129816));
#3465=CARTESIAN_POINT('Ctrl Pts',(0.452578924038324,-23.0756255111136,4.48685838796487));
#3466=CARTESIAN_POINT('Ctrl Pts',(1.12205547802317,-23.1426779051177,4.54415005463158));
#3467=CARTESIAN_POINT('Ctrl Pts',(1.77592690914455,-23.377406537751,4.60144172129822));
#3468=CARTESIAN_POINT('Ctrl Pts',(2.33761535938431,-23.7540489545177,4.65873338796487));
#3469=CARTESIAN_POINT('Ctrl Pts',(2.89930380962407,-24.1306913712844,4.71602505463151));
#3470=CARTESIAN_POINT('Ctrl Pts',(3.36770491189876,-24.6485714795865,4.77331672129828));
#3471=CARTESIAN_POINT('Ctrl Pts',(3.68714965883202,-25.2485638725488,4.83060838796487));
#3472=CARTESIAN_POINT('Ctrl Pts',(4.00659440576528,-25.8485562655112,4.88790005463146));
#3473=CARTESIAN_POINT('Ctrl Pts',(4.17642442602432,-26.5295382611225,4.94519172129826));
#3474=CARTESIAN_POINT('Ctrl Pts',(4.17531508496597,-27.2127225901215,5.00248338796487));
#3475=CARTESIAN_POINT('Ctrl Pts',(4.17420574390762,-27.8959069191205,5.05977505463148));
#3476=CARTESIAN_POINT('Ctrl Pts',(4.00210563848955,-28.579986503623,5.117066721298));
#3477=CARTESIAN_POINT('Ctrl Pts',(3.67744865873987,-29.1850236850955,5.17435838796487));
#3478=CARTESIAN_POINT('Ctrl Pts',(3.35279167899019,-29.790060866568,5.23165005463174));
#3479=CARTESIAN_POINT('Ctrl Pts',(2.8761517580747,-30.3148728474363,5.28894172129792));
#3480=CARTESIAN_POINT('Ctrl Pts',(2.30174618998527,-30.697344184393,5.34623338796487));
#3481=CARTESIAN_POINT('Ctrl Pts',(1.72734062189585,-31.0798155213495,5.40352505463181));
#3482=CARTESIAN_POINT('Ctrl Pts',(1.05623863063331,-31.319169959825,5.46081672129828));
#3483=CARTESIAN_POINT('Ctrl Pts',(0.365925965168119,-31.386045114318,5.51810838796487));
#3484=CARTESIAN_POINT('Ctrl Pts',(-0.324386700297069,-31.4529202688109,
5.57540005463146));
#3485=CARTESIAN_POINT('Ctrl Pts',(-1.03259456986735,-31.3471349250583,5.63269172129805));
#3486=CARTESIAN_POINT('Ctrl Pts',(-1.67611093694732,-31.0793809760956,5.68998338796487));
#3487=CARTESIAN_POINT('Ctrl Pts',(-2.3196273040273,-30.8116270271329,5.74727505463168));
#3488=CARTESIAN_POINT('Ctrl Pts',(-2.89720050000837,-30.3823672928139,5.80456672129819));
#3489=CARTESIAN_POINT('Ctrl Pts',(-3.34070353336454,-29.8402086184987,5.86185838796487));
#3490=CARTESIAN_POINT('Ctrl Pts',(-3.78420656672072,-29.2980499441836,5.91915005463154));
#3491=CARTESIAN_POINT('Ctrl Pts',(-4.09274954484339,-28.643995640032,5.97644172129792));
#3492=CARTESIAN_POINT('Ctrl Pts',(-4.22898613097863,-27.9534017756328,6.03373338796487));
#3493=CARTESIAN_POINT('Ctrl Pts',(-4.36522271711388,-27.2628079112337,6.09102505463182));
#3494=CARTESIAN_POINT('Ctrl Pts',(-4.32883976428306,-26.5369852993421,6.14831672129839));
#3495=CARTESIAN_POINT('Ctrl Pts',(-4.1224436397285,-25.860410023207,6.20560838796487));
#3496=CARTESIAN_POINT('Ctrl Pts',(-3.91604751517394,-25.183834747072,6.26290005463135));
#3497=CARTESIAN_POINT('Ctrl Pts',(-3.53998187857711,-24.5578167789666,6.32019172129842));
#3498=CARTESIAN_POINT('Ctrl Pts',(-3.03657968233749,-24.0559834278915,6.37748338796487));
#3499=CARTESIAN_POINT('Ctrl Pts',(-2.53317748609787,-23.5541500768163,6.43477505463132));
#3500=CARTESIAN_POINT('Ctrl Pts',(-1.90336399926295,-23.1774993067315,6.49206672129798));
#3501=CARTESIAN_POINT('Ctrl Pts',(-1.21953591379696,-22.9712215831745,6.54935838796487));
#3502=CARTESIAN_POINT('Ctrl Pts',(-0.535707828330976,-22.7649438596174,
6.60665005463175));
#3503=CARTESIAN_POINT('Ctrl Pts',(0.200842082192416,-22.7294850572333,6.66394172129835));
#3504=CARTESIAN_POINT('Ctrl Pts',(0.904549975853311,-22.8705923346362,6.72123338796487));
#3505=CARTESIAN_POINT('Ctrl Pts',(1.60825786951421,-23.011699612039,6.77852505463139));
#3506=CARTESIAN_POINT('Ctrl Pts',(2.27776695825421,-23.3291554974211,6.8358167212985));
#3507=CARTESIAN_POINT('Ctrl Pts',(2.83453366104116,-23.7875172137472,6.89310838796487));
#3508=CARTESIAN_POINT('Ctrl Pts',(3.39130036382812,-24.2458789300732,6.95040005463124));
#3509=CARTESIAN_POINT('Ctrl Pts',(3.83422550889456,-24.8443109076698,7.00769172129807));
#3510=CARTESIAN_POINT('Ctrl Pts',(4.11050111787622,-25.5141980776873,7.06498338796487));
#3511=CARTESIAN_POINT('Ctrl Pts',(4.38677672685788,-26.1840852477049,7.12227505463167));
#3512=CARTESIAN_POINT('Ctrl Pts',(4.49582477336048,-26.9241664537426,7.17956672129841));
#3513=CARTESIAN_POINT('Ctrl Pts',(4.42335702191342,-27.6486260546656,7.23685838796487));
#3514=CARTESIAN_POINT('Ctrl Pts',(4.35088927046636,-28.3730856555887,7.29415005463133));
#3515=CARTESIAN_POINT('Ctrl Pts',(4.09699109987682,-29.0805323561617,7.35144172129841));
#3516=CARTESIAN_POINT('Ctrl Pts',(3.68965393532396,-29.6881587428448,7.40873338796487));
#3517=CARTESIAN_POINT('Ctrl Pts',(3.2823167707711,-30.295785129528,7.46602505463132));
#3518=CARTESIAN_POINT('Ctrl Pts',(2.72227543212691,-30.8023989435457,7.52331672129839));
#3519=CARTESIAN_POINT('Ctrl Pts',(2.07355769504457,-31.1478879295178,7.58060838796487));
#3520=CARTESIAN_POINT('Ctrl Pts',(1.42483995796224,-31.4933769154898,7.63790005463135));
#3521=CARTESIAN_POINT('Ctrl Pts',(0.688661729169903,-31.6770328723976,7.69519172129708));
#3522=CARTESIAN_POINT('Ctrl Pts',(-0.0497716862192416,-31.6759235313513,
7.75248338796487));
#3523=CARTESIAN_POINT('Ctrl Pts',(-0.788205101608386,-31.674814190305,7.80977505463266));
#3524=CARTESIAN_POINT('Ctrl Pts',(-1.52748091929412,-31.4888881482022,7.8670667212985));
#3525=CARTESIAN_POINT('Ctrl Pts',(-2.18124344488441,-31.1381869294255,7.92435838796487));
#3526=CARTESIAN_POINT('Ctrl Pts',(-2.83500597047471,-30.7874857106489,7.98165005463124));
#3527=CARTESIAN_POINT('Ctrl Pts',(-3.40197918167131,-30.2726330779668,8.03894172129796));
#3528=CARTESIAN_POINT('Ctrl Pts',(-3.81514526643002,-29.6522895734456,8.09623338796487));
#3529=CARTESIAN_POINT('Ctrl Pts',(-4.22831135118872,-29.0319460689245,8.15352505463178));
#3530=CARTESIAN_POINT('Ctrl Pts',(-4.48683532758525,-28.3072688081897,8.21081672129796));
#3531=CARTESIAN_POINT('Ctrl Pts',(-4.55912583954038,-27.5619730957952,8.26810838796487));
#3532=CARTESIAN_POINT('Ctrl Pts',(-4.63141635149551,-26.8166773834008,8.32540005463178));
#3533=CARTESIAN_POINT('Ctrl Pts',(-4.51728182365348,-26.0521838868124,8.38269172129824));
#3534=CARTESIAN_POINT('Ctrl Pts',(-4.22838496469132,-25.3576240196336,8.43998338796487));
#3535=CARTESIAN_POINT('Ctrl Pts',(-3.93948810572916,-24.6630641524548,8.4972750546315));
#3536=CARTESIAN_POINT('Ctrl Pts',(-3.47633218752116,-24.0397872432635,8.55456672129809));
#3537=CARTESIAN_POINT('Ctrl Pts',(-2.89146539189475,-23.5612345605416,8.61185838796487));
#3538=CARTESIAN_POINT('Ctrl Pts',(-2.30659859626834,-23.0826818778197,8.66915005463165));
#3539=CARTESIAN_POINT('Ctrl Pts',(-1.60110594549964,-22.7498103736324,8.72644172129807));
#3540=CARTESIAN_POINT('Ctrl Pts',(-0.856324590424587,-22.6027952254392,
8.78373338796487));
#3541=CARTESIAN_POINT('Ctrl Pts',(-0.111543235349539,-22.455780077246,8.84102505463166));
#3542=CARTESIAN_POINT('Ctrl Pts',(0.671112336026928,-22.4949550543515,8.89831672129782));
#3543=CARTESIAN_POINT('Ctrl Pts',(1.4005576914376,-22.7173891421077,8.95560838796487));
#3544=CARTESIAN_POINT('Ctrl Pts',(2.13000304684828,-22.9398232298639,9.01290005463192));
#3545=CARTESIAN_POINT('Ctrl Pts',(2.80482705930729,-23.3451420836895,9.07019172129816));
#3546=CARTESIAN_POINT('Ctrl Pts',(3.34572741401944,-23.8876112835564,9.12748338796487));
#3547=CARTESIAN_POINT('Ctrl Pts',(3.88662776873157,-24.4300804834233,9.18477505463157));
#3548=CARTESIAN_POINT('Ctrl Pts',(4.292531756023,-25.1087000146355,9.24206672129765));
#3549=CARTESIAN_POINT('Ctrl Pts',(4.51484744279408,-25.8453981793633,9.29935838796487));
#3550=CARTESIAN_POINT('Ctrl Pts',(4.73716312956515,-26.582096344091,9.35665005463209));
#3551=CARTESIAN_POINT('Ctrl Pts',(4.77541395619357,-27.3754792141155,9.4139417212973));
#3552=CARTESIAN_POINT('Ctrl Pts',(4.6235281167506,-28.1333745984499,9.47123338796487));
#3553=CARTESIAN_POINT('Ctrl Pts',(4.47164227730762,-28.8912699827844,9.52852505463244));
#3554=CARTESIAN_POINT('Ctrl Pts',(4.12985786582675,-29.6122174181468,9.58581672129756));
#3555=CARTESIAN_POINT('Ctrl Pts',(3.63644650015124,-30.211692242242,9.64310838796487));
#3556=CARTESIAN_POINT('Ctrl Pts',(3.14303513447573,-30.8111670663372,9.70040005463217));
#3557=CARTESIAN_POINT('Ctrl Pts',(2.49889944364267,-31.2879883952817,9.7576917212976));
#3558=CARTESIAN_POINT('Ctrl Pts',(1.77796877353627,-31.5854069142767,9.81498338796487));
#3559=CARTESIAN_POINT('Ctrl Pts',(1.05703810342986,-31.8828254332717,9.87227505463214));
#3560=CARTESIAN_POINT('Ctrl Pts',(0.260671270356954,-32.0002226638335,9.92956672129819));
#3561=CARTESIAN_POINT('Ctrl Pts',(-0.518771377488306,-31.9223395549405,
9.98685838796487));
#3562=CARTESIAN_POINT('Ctrl Pts',(-1.29821402533357,-31.8444564460475,10.0441500546315));
#3563=CARTESIAN_POINT('Ctrl Pts',(-2.05923599538643,-31.5713887375034,10.1014417212983));
#3564=CARTESIAN_POINT('Ctrl Pts',(-2.71280031850067,-31.1333568251656,10.1587333879649));
#3565=CARTESIAN_POINT('Ctrl Pts',(-3.36636464161491,-30.6953249128279,10.2160250546314));
#3566=CARTESIAN_POINT('Ctrl Pts',(-3.91119116738902,-30.0931223438177,10.2733167212985));
#3567=CARTESIAN_POINT('Ctrl Pts',(-4.28272439239882,-29.395679262638,10.3306083879649));
#3568=CARTESIAN_POINT('Ctrl Pts',(-4.65425761740862,-28.6982361814583,10.3879000546312));
#3569=CARTESIAN_POINT('Ctrl Pts',(-4.85173820194801,-27.9068617491303,10.445191722014));
#3570=CARTESIAN_POINT('Ctrl Pts',(-4.85063030442627,-27.1131792193187,10.5024833878013));
#3571=CARTESIAN_POINT('Origin',(-4.85063016993195,-27.162950903902,11.));
#3572=CARTESIAN_POINT('Ctrl Pts',(-3.5,-27.2127225901214,0.49751661203513));
#3573=CARTESIAN_POINT('Ctrl Pts',(-3.51517840571961,-26.6400364200585,0.554808278701816));
#3574=CARTESIAN_POINT('Ctrl Pts',(-3.3870023381626,-26.0622733505101,0.612099945368435));
#3575=CARTESIAN_POINT('Ctrl Pts',(-3.12879834611319,-25.5470088669697,0.66939161203513));
#3576=CARTESIAN_POINT('Ctrl Pts',(-2.87059435406378,-25.0317443834292,0.726683278701825));
#3577=CARTESIAN_POINT('Ctrl Pts',(-2.48280922845853,-24.5799895371609,0.78397494536851));
#3578=CARTESIAN_POINT('Ctrl Pts',(-2.00932852015756,-24.2453649299115,0.84126661203513));
#3579=CARTESIAN_POINT('Ctrl Pts',(-1.5358478118566,-23.9107403226621,0.89855827870175));
#3580=CARTESIAN_POINT('Ctrl Pts',(-0.9775476488716,-23.6939306641498,0.955849945368433));
#3581=CARTESIAN_POINT('Ctrl Pts',(-0.398797555610286,-23.6216769084413,
1.01314161203513));
#3582=CARTESIAN_POINT('Ctrl Pts',(0.179952537651027,-23.5494231527329,1.07043327870183));
#3583=CARTESIAN_POINT('Ctrl Pts',(0.778050540497908,-23.6219168035854,1.12772494536847));
#3584=CARTESIAN_POINT('Ctrl Pts',(1.3257129579118,-23.8323370172714,1.18501661203513));
#3585=CARTESIAN_POINT('Ctrl Pts',(1.8733753753257,-24.0427572309574,1.24230827870179));
#3586=CARTESIAN_POINT('Ctrl Pts',(2.36953393381726,-24.3907508815125,1.29959994536854));
#3587=CARTESIAN_POINT('Ctrl Pts',(2.75552826641451,-24.837160476445,1.35689161203513));
#3588=CARTESIAN_POINT('Ctrl Pts',(3.14152259901176,-25.2835700713775,1.41418327870172));
#3589=CARTESIAN_POINT('Ctrl Pts',(3.41657284380058,-25.8275754937386,1.47147494536833));
#3590=CARTESIAN_POINT('Ctrl Pts',(3.54722708742622,-26.4066167951111,1.52876661203513));
#3591=CARTESIAN_POINT('Ctrl Pts',(3.67788133105185,-26.9856580964837,1.58605827870193));
#3592=CARTESIAN_POINT('Ctrl Pts',(3.6638371082595,-27.5986378942041,1.64334994536846));
#3593=CARTESIAN_POINT('Ctrl Pts',(3.50510331133718,-28.1742010948723,1.70064161203513));
#3594=CARTESIAN_POINT('Ctrl Pts',(3.34636951441486,-28.7497642955405,1.7579332787018));
#3595=CARTESIAN_POINT('Ctrl Pts',(3.04319861323196,-29.2867941907393,1.81522494536844));
#3596=CARTESIAN_POINT('Ctrl Pts',(2.62944759999372,-29.7220107102229,1.87251661203513));
#3597=CARTESIAN_POINT('Ctrl Pts',(2.21569658675549,-30.1572272297066,1.92980827870182));
#3598=CARTESIAN_POINT('Ctrl Pts',(1.69211920432461,-30.4897598664222,1.98709994536844));
#3599=CARTESIAN_POINT('Ctrl Pts',(1.11875936055348,-30.6795480647568,2.04439161203513));
#3600=CARTESIAN_POINT('Ctrl Pts',(0.545399516782366,-30.8693362630914,2.10168327870182));
#3601=CARTESIAN_POINT('Ctrl Pts',(-0.0766613701186385,-30.9159656984605,
2.15897494536837));
#3602=CARTESIAN_POINT('Ctrl Pts',(-0.67517186401586,-30.8123903267832,2.21626661203513));
#3603=CARTESIAN_POINT('Ctrl Pts',(-1.27368235791308,-30.7088149551059,2.27355827870189));
#3604=CARTESIAN_POINT('Ctrl Pts',(-1.84748694212142,-30.4551804406305,2.33084994536844));
#3605=CARTESIAN_POINT('Ctrl Pts',(-2.32917023898663,-30.0795086210231,2.38814161203513));
#3606=CARTESIAN_POINT('Ctrl Pts',(-2.81085353585185,-29.7038368014157,2.44543327870183));
#3607=CARTESIAN_POINT('Ctrl Pts',(-3.19946002926004,-29.2068050390794,2.50272494536839));
#3608=CARTESIAN_POINT('Ctrl Pts',(-3.44849773344619,-28.6452379198675,2.56001661203513));
#3609=CARTESIAN_POINT('Ctrl Pts',(-3.69753543763233,-28.0836708006555,2.61730827870187));
#3610=CARTESIAN_POINT('Ctrl Pts',(-3.80647844076847,-27.458622235808,2.67459994536845));
#3611=CARTESIAN_POINT('Ctrl Pts',(-3.76105072036911,-26.8425322504808,2.73189161203513));
#3612=CARTESIAN_POINT('Ctrl Pts',(-3.71562299996974,-26.2264422651536,2.7891832787018));
#3613=CARTESIAN_POINT('Ctrl Pts',(-3.51585820108909,-25.6204948140464,2.84647494536852));
#3614=CARTESIAN_POINT('Ctrl Pts',(-3.18345329806631,-25.0956953133645,2.90376661203513));
#3615=CARTESIAN_POINT('Ctrl Pts',(-2.85104839504354,-24.5708958126827,2.96105827870174));
#3616=CARTESIAN_POINT('Ctrl Pts',(-2.38659484300895,-24.1282780503191,3.01834994536843));
#3617=CARTESIAN_POINT('Ctrl Pts',(-1.84300578454046,-23.8205130327937,3.07564161203513));
#3618=CARTESIAN_POINT('Ctrl Pts',(-1.29941672607197,-23.5127480152682,3.13293327870183));
#3619=CARTESIAN_POINT('Ctrl Pts',(-0.677706928819807,-23.3404717664636,
3.19022494536847));
#3620=CARTESIAN_POINT('Ctrl Pts',(-0.0497716862189807,-23.3252933614193,
3.24751661203513));
#3621=CARTESIAN_POINT('Ctrl Pts',(0.578163556381841,-23.3101149563751,3.30480827870179));
#3622=CARTESIAN_POINT('Ctrl Pts',(1.21112287292379,-23.4521169599317,3.3620999453685));
#3623=CARTESIAN_POINT('Ctrl Pts',(1.77511270062386,-23.7363651910058,3.41939161203513));
#3624=CARTESIAN_POINT('Ctrl Pts',(2.33910252832392,-24.02061342208,3.47668327870176));
#3625=CARTESIAN_POINT('Ctrl Pts',(2.83301860484105,-24.4466112594378,3.53397494536822));
#3626=CARTESIAN_POINT('Ctrl Pts',(3.19833795993023,-24.9660299041867,3.59126661203513));
#3627=CARTESIAN_POINT('Ctrl Pts',(3.56365731501942,-25.4854485489357,3.64855827870204));
#3628=CARTESIAN_POINT('Ctrl Pts',(3.79963651139122,-26.0973239813465,3.70584994536859));
#3629=CARTESIAN_POINT('Ctrl Pts',(3.87730562458575,-26.7310571215672,3.76314161203513));
#3630=CARTESIAN_POINT('Ctrl Pts',(3.95497473778028,-27.364790261788,3.82043327870167));
#3631=CARTESIAN_POINT('Ctrl Pts',(3.87413190281369,-28.0191738915788,3.87772494536818));
#3632=CARTESIAN_POINT('Ctrl Pts',(3.64256877912899,-28.6178798091356,3.93501661203513));
#3633=CARTESIAN_POINT('Ctrl Pts',(3.41100565544429,-29.2165857266924,3.99230827870208));
#3634=CARTESIAN_POINT('Ctrl Pts',(3.02911582100773,-29.7584479983173,4.04959994536851));
#3635=CARTESIAN_POINT('Ctrl Pts',(2.53999810475567,-30.179491980313,4.10689161203513));
#3636=CARTESIAN_POINT('Ctrl Pts',(2.05088038850359,-30.6005359623087,4.16418327870175));
#3637=CARTESIAN_POINT('Ctrl Pts',(1.45543661955603,-30.8999147331016,4.22147494536847));
#3638=CARTESIAN_POINT('Ctrl Pts',(0.822207827485342,-31.041347538813,4.27876661203513));
#3639=CARTESIAN_POINT('Ctrl Pts',(0.188979035414649,-31.1827803445244,4.33605827870178));
#3640=CARTESIAN_POINT('Ctrl Pts',(-0.480833721736333,-31.1659440974169,
4.39334994536825));
#3641=CARTESIAN_POINT('Ctrl Pts',(-1.10926700171223,-30.9911723373057,4.45064161203513));
#3642=CARTESIAN_POINT('Ctrl Pts',(-1.73770028168812,-30.8164005771944,4.50793327870201));
#3643=CARTESIAN_POINT('Ctrl Pts',(-2.32353622117369,-30.4839764587754,4.56522494536848));
#3644=CARTESIAN_POINT('Ctrl Pts',(-2.79781974432916,-30.0311584419045,4.62251661203513));
#3645=CARTESIAN_POINT('Ctrl Pts',(-3.27210326748465,-29.5783404250336,4.67980827870178));
#3646=CARTESIAN_POINT('Ctrl Pts',(-3.63388912134312,-29.0059569982611,4.73709994536835));
#3647=CARTESIAN_POINT('Ctrl Pts',(-3.83971528292067,-28.379727075198,4.79439161203513));
#3648=CARTESIAN_POINT('Ctrl Pts',(-4.04554144449821,-27.7534971521348,4.85168327870191));
#3649=CARTESIAN_POINT('Ctrl Pts',(-4.09496290407286,-27.0746033058008,4.90897494536821));
#3650=CARTESIAN_POINT('Ctrl Pts',(-3.98060897036527,-26.4219053211922,4.96626661203513));
#3651=CARTESIAN_POINT('Ctrl Pts',(-3.86625503665767,-25.7692073365837,5.02355827870204));
#3652=CARTESIAN_POINT('Ctrl Pts',(-3.58829199607698,-25.1439644058301,5.08084994536843));
#3653=CARTESIAN_POINT('Ctrl Pts',(-3.17757052711683,-24.6195729876172,5.13814161203513));
#3654=CARTESIAN_POINT('Ctrl Pts',(-2.76684905815666,-24.0951815694043,5.19543327870183));
#3655=CARTESIAN_POINT('Ctrl Pts',(-2.22411358260874,-23.6726788921877,5.25272494536842));
#3656=CARTESIAN_POINT('Ctrl Pts',(-1.61150296328641,-23.402498277958,5.31001661203513));
#3657=CARTESIAN_POINT('Ctrl Pts',(-0.998892343964086,-23.1323176637283,
5.36730827870184));
#3658=CARTESIAN_POINT('Ctrl Pts',(-0.317558152137085,-23.0150254765812,
5.42459994536842));
#3659=CARTESIAN_POINT('Ctrl Pts',(0.353514880146535,-23.0658685544085,5.48189161203513));
#3660=CARTESIAN_POINT('Ctrl Pts',(1.02458791243016,-23.1167116322358,5.53918327870184));
#3661=CARTESIAN_POINT('Ctrl Pts',(1.68411063294507,-23.3356459690878,5.59647494536849));
#3662=CARTESIAN_POINT('Ctrl Pts',(2.25484807009596,-23.6987456198967,5.65376661203513));
#3663=CARTESIAN_POINT('Ctrl Pts',(2.82558550724686,-24.0618452707057,5.71105827870177));
#3664=CARTESIAN_POINT('Ctrl Pts',(3.30641598130079,-24.5684600530816,5.76834994536854));
#3665=CARTESIAN_POINT('Ctrl Pts',(3.64022523789207,-25.1607744556708,5.82564161203513));
#3666=CARTESIAN_POINT('Ctrl Pts',(3.97403449448334,-25.75308885826,5.88293327870172));
#3667=CARTESIAN_POINT('Ctrl Pts',(4.16013667989657,-26.4299948886844,5.94022494536852));
#3668=CARTESIAN_POINT('Ctrl Pts',(4.17531508496597,-27.1131792176834,5.99751661203513));
#3669=CARTESIAN_POINT('Ctrl Pts',(4.19049349003537,-27.7963635466825,6.05480827870174));
#3670=CARTESIAN_POINT('Ctrl Pts',(4.03466554977154,-28.4845190963707,6.11209994536826));
#3671=CARTESIAN_POINT('Ctrl Pts',(3.72437307967983,-29.0972342682174,6.16939161203513));
#3672=CARTESIAN_POINT('Ctrl Pts',(3.41408060958811,-29.7099494400641,6.226683278702));
#3673=CARTESIAN_POINT('Ctrl Pts',(2.94987006045165,-30.2460267468577,6.28397494536819));
#3674=CARTESIAN_POINT('Ctrl Pts',(2.38451347927363,-30.642040849772,6.34126661203513));
#3675=CARTESIAN_POINT('Ctrl Pts',(1.81915689809562,-31.0380549526863,6.39855827870207));
#3676=CARTESIAN_POINT('Ctrl Pts',(1.15370619622606,-31.2932036869398,6.45584994536854));
#3677=CARTESIAN_POINT('Ctrl Pts',(0.46499000905991,-31.3762881576128,6.51314161203513));
#3678=CARTESIAN_POINT('Ctrl Pts',(-0.223726178106243,-31.4593726282858,
6.57043327870172));
#3679=CARTESIAN_POINT('Ctrl Pts',(-0.934395434881118,-31.3701806092124,
6.62772494536832));
#3680=CARTESIAN_POINT('Ctrl Pts',(-1.58414485255466,-31.1174745755294,6.68501661203513));
#3681=CARTESIAN_POINT('Ctrl Pts',(-2.2338942702282,-30.8647685418463,6.74230827870194));
#3682=CARTESIAN_POINT('Ctrl Pts',(-2.82146025502991,-30.4489825235109,6.79959994536846));
#3683=CARTESIAN_POINT('Ctrl Pts',(-3.27755388640684,-29.9171566859563,6.85689161203513));
#3684=CARTESIAN_POINT('Ctrl Pts',(-3.73364751778377,-29.3853308484018,6.9141832787018));
#3685=CARTESIAN_POINT('Ctrl Pts',(-4.05735481460304,-28.7384487328433,6.97147494536818));
#3686=CARTESIAN_POINT('Ctrl Pts',(-4.20956618239513,-28.0510324500818,7.02876661203513));
#3687=CARTESIAN_POINT('Ctrl Pts',(-4.36177755018722,-27.3636161673202,7.08605827870208));
#3688=CARTESIAN_POINT('Ctrl Pts',(-4.34214927877063,-26.6369704507106,7.14334994536865));
#3689=CARTESIAN_POINT('Ctrl Pts',(-4.15133955546951,-25.9556670914478,7.20064161203513));
#3690=CARTESIAN_POINT('Ctrl Pts',(-3.96052983216839,-25.2743637321851,7.25793327870161));
#3691=CARTESIAN_POINT('Ctrl Pts',(-3.59885249650757,-24.6397217483839,7.31522494536868));
#3692=CARTESIAN_POINT('Ctrl Pts',(-3.10696747601062,-24.1263712215646,7.37251661203513));
#3693=CARTESIAN_POINT('Ctrl Pts',(-2.61508245551368,-23.6130206947453,7.42980827870158));
#3694=CARTESIAN_POINT('Ctrl Pts',(-1.99389298437356,-23.2219816237259,7.48709994536824));
#3695=CARTESIAN_POINT('Ctrl Pts',(-1.31479298203775,-23.0001174989155,7.54439161203513));
#3696=CARTESIAN_POINT('Ctrl Pts',(-0.635692979701941,-22.778253374105,7.60168327870201));
#3697=CARTESIAN_POINT('Ctrl Pts',(0.100033826104315,-22.7260398903107,7.65897494536861));
#3698=CARTESIAN_POINT('Ctrl Pts',(0.806919301404371,-22.8511723860526,7.71626661203513));
#3699=CARTESIAN_POINT('Ctrl Pts',(1.51380477670443,-22.9763048817946,7.77355827870165));
#3700=CARTESIAN_POINT('Ctrl Pts',(2.19048605403487,-23.2785964484885,7.83084994536837));
#3701=CARTESIAN_POINT('Ctrl Pts',(2.75758559358357,-23.7243675667894,7.88814161203513));
#3702=CARTESIAN_POINT('Ctrl Pts',(3.32468513313228,-24.1701386850904,7.94543327870189));
#3703=CARTESIAN_POINT('Ctrl Pts',(3.7810839941741,-24.758577873874,8.00272494536833));
#3704=CARTESIAN_POINT('Ctrl Pts',(4.07240751844243,-25.4222319932947,8.06001661203513));
#3705=CARTESIAN_POINT('Ctrl Pts',(4.36373104271076,-26.0858861127153,8.11730827870193));
#3706=CARTESIAN_POINT('Ctrl Pts',(4.48937241387869,-26.8235059315532,8.17459994536906));
#3707=CARTESIAN_POINT('Ctrl Pts',(4.43311397861856,-27.5495620107739,8.23189161203513));
#3708=CARTESIAN_POINT('Ctrl Pts',(4.37685554335844,-28.2756180899945,8.28918327870121));
#3709=CARTESIAN_POINT('Ctrl Pts',(4.13875166853063,-28.9887160799575,8.34647494536867));
#3710=CARTESIAN_POINT('Ctrl Pts',(3.74495726994493,-29.6053914535565,8.40376661203513));
#3711=CARTESIAN_POINT('Ctrl Pts',(3.35116287135924,-30.2220668271555,8.46105827870158));
#3712=CARTESIAN_POINT('Ctrl Pts',(2.80238685862471,-30.7411100129369,8.51834994536943));
#3713=CARTESIAN_POINT('Ctrl Pts',(2.16134711192264,-31.1009635085778,8.57564161203513));
#3714=CARTESIAN_POINT('Ctrl Pts',(1.52030736522058,-31.4608170042187,8.63293327870082));
#3715=CARTESIAN_POINT('Ctrl Pts',(0.788205101607957,-31.6607451262615,8.69022494536734));
#3716=CARTESIAN_POINT('Ctrl Pts',(0.0497716862188113,-31.6759235313513,
8.74751661203513));
#3717=CARTESIAN_POINT('Ctrl Pts',(-0.688661729170334,-31.6911019364411,
8.80480827870292));
#3718=CARTESIAN_POINT('Ctrl Pts',(-1.43201351203358,-31.521448059472,8.86209994536876));
#3719=CARTESIAN_POINT('Ctrl Pts',(-2.09345402800635,-31.1851113503655,8.91939161203513));
#3720=CARTESIAN_POINT('Ctrl Pts',(-2.75489454397912,-30.848774641259,8.9766832787015));
#3721=CARTESIAN_POINT('Ctrl Pts',(-3.33313308108255,-30.3463513803362,9.03397494536822));
#3722=CARTESIAN_POINT('Ctrl Pts',(-3.75984193180906,-29.735056862734,9.09126661203513));
#3723=CARTESIAN_POINT('Ctrl Pts',(-4.18655078253556,-29.1237623451318,9.14855827870204));
#3724=CARTESIAN_POINT('Ctrl Pts',(-4.46086905468824,-28.404736373781,9.20584994536822));
#3725=CARTESIAN_POINT('Ctrl Pts',(-4.54936888283525,-27.661037139687,9.26314161203513));
#3726=CARTESIAN_POINT('Ctrl Pts',(-4.63786871098225,-26.9173379055931,9.32043327870204));
#3727=CARTESIAN_POINT('Ctrl Pts',(-4.54032750779717,-26.1503830218042,9.3777249453685));
#3728=CARTESIAN_POINT('Ctrl Pts',(-4.26647856412511,-25.4495901040262,9.43501661203513));
#3729=CARTESIAN_POINT('Ctrl Pts',(-3.99262962045306,-24.7487971862483,9.49230827870176));
#3730=CARTESIAN_POINT('Ctrl Pts',(-3.54294741821143,-24.1155274882508,9.54959994536835));
#3731=CARTESIAN_POINT('Ctrl Pts',(-2.96841345935235,-23.6243842074993,9.60689161203513));
#3732=CARTESIAN_POINT('Ctrl Pts',(-2.39387950049327,-23.1332409267478,9.66418327870191));
#3733=CARTESIAN_POINT('Ctrl Pts',(-1.69555903830894,-22.7852051038845,9.72147494536834));
#3734=CARTESIAN_POINT('Ctrl Pts',(-0.953955264873529,-22.6222151740227,
9.77876661203513));
#3735=CARTESIAN_POINT('Ctrl Pts',(-0.212351491438118,-22.4592252441609,
9.83605827870193));
#3736=CARTESIAN_POINT('Ctrl Pts',(0.571127184652931,-22.4816455398733,9.89334994536808));
#3737=CARTESIAN_POINT('Ctrl Pts',(1.30530062319683,-22.6884932263666,9.95064161203513));
#3738=CARTESIAN_POINT('Ctrl Pts',(2.03947406174072,-22.89534091286,10.0079332787022));
#3739=CARTESIAN_POINT('Ctrl Pts',(2.72292208988536,-23.2862714657652,10.0652249453684));
#3740=CARTESIAN_POINT('Ctrl Pts',(3.27533962034631,-23.8172234898833,10.1225166120351));
#3741=CARTESIAN_POINT('Ctrl Pts',(3.82775715080726,-24.3481755140014,10.1798082787018));
#3742=CARTESIAN_POINT('Ctrl Pts',(4.24804943901783,-25.0181710295281,10.2370999453679));
#3743=CARTESIAN_POINT('Ctrl Pts',(4.48595152705308,-25.7501411111225,10.2943916120351));
#3744=CARTESIAN_POINT('Ctrl Pts',(4.72385361508833,-26.4821111927169,10.3516832787023));
#3745=CARTESIAN_POINT('Ctrl Pts',(4.7788591231067,-27.2746709580248,10.4089749453667));
#3746=CARTESIAN_POINT('Ctrl Pts',(4.64294806533411,-28.035743924001,10.4662666120351));
#3747=CARTESIAN_POINT('Ctrl Pts',(4.50703700756152,-28.7968168899771,10.5235582787035));
#3748=CARTESIAN_POINT('Ctrl Pts',(4.18041691475187,-29.5249365139219,10.5808499453678));
#3749=CARTESIAN_POINT('Ctrl Pts',(3.69959614710895,-30.1347441747844,10.6381416120351));
#3750=CARTESIAN_POINT('Ctrl Pts',(3.21877537946604,-30.7445518356469,10.6954332787024));
#3751=CARTESIAN_POINT('Ctrl Pts',(2.58463247743366,-31.2348468805496,10.7527249453679));
#3752=CARTESIAN_POINT('Ctrl Pts',(1.86993485792894,-31.5473133148429,10.8100166120351));
#3753=CARTESIAN_POINT('Ctrl Pts',(1.15523723842421,-31.8597797491362,10.8673082787024));
#3754=CARTESIAN_POINT('Ctrl Pts',(0.361331792548353,-31.9937703043426,10.9245999453685));
#3755=CARTESIAN_POINT('Ctrl Pts',(-0.419707333596513,-31.9320965116456,
10.9818916120351));
#3756=CARTESIAN_POINT('Ctrl Pts',(-1.20074645974138,-31.8704227189487,11.0391832787018));
#3757=CARTESIAN_POINT('Ctrl Pts',(-1.96741971917488,-31.613149306151,11.0964749453686));
#3758=CARTESIAN_POINT('Ctrl Pts',(-2.63003302921232,-31.1886601597866,11.1537666120351));
#3759=CARTESIAN_POINT('Ctrl Pts',(-3.29264633924977,-30.7641710134222,11.2110582787017));
#3760=CARTESIAN_POINT('Ctrl Pts',(-3.84990223677302,-30.1732337703105,11.2683499453688));
#3761=CARTESIAN_POINT('Ctrl Pts',(-4.23579997145888,-29.4834686795161,11.3256416120351));
#3762=CARTESIAN_POINT('Ctrl Pts',(-4.62169770614474,-28.7937035887216,11.3829332787015));
#3763=CARTESIAN_POINT('Ctrl Pts',(-4.83545289018665,-28.0064050826244,11.4402249455077));
#3764=CARTESIAN_POINT('Ctrl Pts',(-4.85063010478977,-27.2127235347731,11.4975165438617));
#3765=CARTESIAN_POINT('Ctrl Pts',(-3.49999867141204,-27.1131792015256,-0.497516610416937));
#3766=CARTESIAN_POINT('Ctrl Pts',(-3.49888932799759,-26.5404932488512,-0.440224943750252));
#3767=CARTESIAN_POINT('Ctrl Pts',(-3.35444114738347,-25.9668063623456,-0.382933277083632));
#3768=CARTESIAN_POINT('Ctrl Pts',(-2.80930434430968,-24.9516337619221,-0.268349943750243));
#3769=CARTESIAN_POINT('Ctrl Pts',(-2.40908999522195,-24.5111444093371,-0.211058277083598));
#3770=CARTESIAN_POINT('Ctrl Pts',(-1.44403096339936,-23.8689809726516,-0.0964749437502769));
#3771=CARTESIAN_POINT('Ctrl Pts',(-0.880079720887058,-23.6679656879623,
-0.0391832770835939));
#3772=CARTESIAN_POINT('Ctrl Pts',(0.28061299005863,-23.5558768567235,0.0754000562497192));
#3773=CARTESIAN_POINT('Ctrl Pts',(0.876249383825206,-23.6449638021555,0.132691722916406));
#3774=CARTESIAN_POINT('Ctrl Pts',(1.95910771378206,-24.0958998985319,0.247275056249719));
#3775=CARTESIAN_POINT('Ctrl Pts',(2.44527330196474,-24.4573671339349,0.304566722916428));
#3776=CARTESIAN_POINT('Ctrl Pts',(3.19208049125558,-25.370851664545,0.419150056249697));
#3777=CARTESIAN_POINT('Ctrl Pts',(3.4519663191088,-25.9220290742938,0.476441722916301));
#3778=CARTESIAN_POINT('Ctrl Pts',(3.68132515309603,-27.08646641491,0.591025056249824));
#3779=CARTESIAN_POINT('Ctrl Pts',(3.65052625709869,-27.6986228841538,0.648316722916396));
#3780=CARTESIAN_POINT('Ctrl Pts',(3.30188598195419,-28.8402927016588,0.762900056249729));
#3781=CARTESIAN_POINT('Ctrl Pts',(2.98432689255302,-29.3686983876925,0.820191722916372));
#3782=CARTESIAN_POINT('Ctrl Pts',(2.13379081833063,-30.216096764043,0.934775056249753));
#3783=CARTESIAN_POINT('Ctrl Pts',(1.60158961081322,-30.5342409823362,0.992066722916289));
#3784=CARTESIAN_POINT('Ctrl Pts',(0.445414171550833,-30.8826444452813,1.10665005624984));
#3785=CARTESIAN_POINT('Ctrl Pts',(-0.177469596581333,-30.912519185481,1.16394172291647));
#3786=CARTESIAN_POINT('Ctrl Pts',(-1.36813499365341,-30.6734189584949,1.27852505624965));
#3787=CARTESIAN_POINT('Ctrl Pts',(-1.93476718568864,-30.4046202185468,1.33581672291637));
#3788=CARTESIAN_POINT('Ctrl Pts',(-2.87746776648538,-29.6280956550586,1.45040005624976));
#3789=CARTESIAN_POINT('Ctrl Pts',(-3.25260040831661,-29.1210712820873,1.50769172291632));
#3790=CARTESIAN_POINT('Ctrl Pts',(-3.72057981489945,-27.9854713421496,1.6222750562498));
#3791=CARTESIAN_POINT('Ctrl Pts',(-3.81292945777313,-27.3579616111638,1.67956672291639));
#3792=CARTESIAN_POINT('Ctrl Pts',(-3.68965542200644,-26.1289750303032,1.79415005624974));
#3793=CARTESIAN_POINT('Ctrl Pts',(-3.47409640017873,-25.5286790803258,1.85144172291645));
#3794=CARTESIAN_POINT('Ctrl Pts',(-2.78220129939746,-24.4971784172052,1.96602505624967));
#3795=CARTESIAN_POINT('Ctrl Pts',(-2.30648258548237,-24.0669901790178,2.02331672291636));
#3796=CARTESIAN_POINT('Ctrl Pts',(-1.20394886875872,-23.4801893728762,2.13790005624977));
#3797=CARTESIAN_POINT('Ctrl Pts',(-0.578163322834367,-23.3241853462944,
2.1951917229164));
#3798=CARTESIAN_POINT('Ctrl Pts',(0.677706727587892,-23.3264040337203,2.30977505624973));
#3799=CARTESIAN_POINT('Ctrl Pts',(1.30658986109621,-23.4846781506972,2.36706672291644));
#3800=CARTESIAN_POINT('Ctrl Pts',(2.4192131498232,-24.0819034318477,2.48165005624969));
#3801=CARTESIAN_POINT('Ctrl Pts',(2.9018637326796,-24.5203304926646,2.53894172291615));
#3802=CARTESIAN_POINT('Ctrl Pts',(3.60541666501523,-25.5772653974027,2.65352505624997));
#3803=CARTESIAN_POINT('Ctrl Pts',(3.82560148759511,-26.1947919093305,2.71081672291652));
#3804=CARTESIAN_POINT('Ctrl Pts',(3.94852103377322,-27.4654507141961,2.8254000562496));
#3805=CARTESIAN_POINT('Ctrl Pts',(3.85108490425945,-28.1173727349135,2.88269172291611));
#3806=CARTESIAN_POINT('Ctrl Pts',(3.35786298785392,-29.3023180651413,2.99727505625001));
#3807=CARTESIAN_POINT('Ctrl Pts',(2.96249956859728,-29.8341873664785,3.05456672291645));
#3808=CARTESIAN_POINT('Ctrl Pts',(1.96359879532417,-30.6510938545388,3.16915005624968));
#3809=CARTESIAN_POINT('Ctrl Pts',(1.36098303900346,-30.9353082084263,3.22644172291641));
#3810=CARTESIAN_POINT('Ctrl Pts',(0.0881707169855854,-31.1862241665521,
3.34102505624972));
#3811=CARTESIAN_POINT('Ctrl Pts',(-0.580818711692515,-31.1526332462716,
3.39831672291618));
#3812=CARTESIAN_POINT('Ctrl Pts',(-1.82822868779995,-30.7719170447183,3.51290005624994));
#3813=CARTESIAN_POINT('Ctrl Pts',(-2.40544041813704,-30.4251047381095,3.57019172291641));
#3814=CARTESIAN_POINT('Ctrl Pts',(-3.33097280181086,-29.4964346565957,3.68477505624972));
#3815=CARTESIAN_POINT('Ctrl Pts',(-3.67837023727213,-28.9154274047545,3.74206672291629));
#3816=CARTESIAN_POINT('Ctrl Pts',(-4.05884962667304,-27.6535118068985,3.85665005624984));
#3817=CARTESIAN_POINT('Ctrl Pts',(-4.09151639110769,-26.9737950793345,3.91394172291615));
#3818=CARTESIAN_POINT('Ctrl Pts',(-3.83085904003235,-25.6747547008469,4.02852505624998));
#3819=CARTESIAN_POINT('Ctrl Pts',(-3.53773177400349,-25.0566841622527,4.08581672291636));
#3820=CARTESIAN_POINT('Ctrl Pts',(-2.69110791178932,-24.028567338781,4.20040005624976));
#3821=CARTESIAN_POINT('Ctrl Pts',(-2.13837982562106,-23.6195385131152,4.25769172291635));
#3822=CARTESIAN_POINT('Ctrl Pts',(-0.900692885453703,-23.1092732864771,
4.37227505624977));
#3823=CARTESIAN_POINT('Ctrl Pts',(-0.216897527488987,-23.0085744595606,
4.42956672291635));
#3824=CARTESIAN_POINT('Ctrl Pts',(1.12205514727662,-23.142679210215,4.54415005624977));
#3825=CARTESIAN_POINT('Ctrl Pts',(1.775926366677,-23.3774077699852,4.60144172291642));
#3826=CARTESIAN_POINT('Ctrl Pts',(2.89930290271304,-24.1306923663646,4.71602505624971));
#3827=CARTESIAN_POINT('Ctrl Pts',(3.36770385261388,-24.6485723106026,4.77331672291647));
#3828=CARTESIAN_POINT('Ctrl Pts',(4.00659313686357,-25.8485567155787,4.88790005624965));
#3829=CARTESIAN_POINT('Ctrl Pts',(4.17642310008015,-26.5295384946699,4.94519172291645));
#3830=CARTESIAN_POINT('Ctrl Pts',(4.17420441267586,-27.8959067178885,5.05977505624967));
#3831=CARTESIAN_POINT('Ctrl Pts',(4.00210435901772,-28.5799860845476,5.11706672291619));
#3832=CARTESIAN_POINT('Ctrl Pts',(3.3527905998087,-29.7900600615589,5.23165005624993));
#3833=CARTESIAN_POINT('Ctrl Pts',(2.87615082723203,-30.314871874706,5.28894172291612));
#3834=CARTESIAN_POINT('Ctrl Pts',(1.72734004962141,-31.0798143026723,5.40352505625001));
#3835=CARTESIAN_POINT('Ctrl Pts',(1.05623826824525,-31.3191686631573,5.46081672291647));
#3836=CARTESIAN_POINT('Ctrl Pts',(-0.324386630517576,-31.4529189242652,
5.57540005624965));
#3837=CARTESIAN_POINT('Ctrl Pts',(-1.03259427822014,-31.3471336106709,5.63269172291625));
#3838=CARTESIAN_POINT('Ctrl Pts',(-2.31962660867283,-30.8116258742433,5.74727505624988));
#3839=CARTESIAN_POINT('Ctrl Pts',(-2.89719962320057,-30.3823662711092,5.80456672291639));
#3840=CARTESIAN_POINT('Ctrl Pts',(-3.78420541000443,-29.2980492552136,5.91915005624974));
#3841=CARTESIAN_POINT('Ctrl Pts',(-4.09274828993971,-28.6439951522933,5.97644172291612));
#3842=CARTESIAN_POINT('Ctrl Pts',(-4.36522137220295,-27.2628078488887,6.09102505625001));
#3843=CARTESIAN_POINT('Ctrl Pts',(-4.32883842763837,-26.5369854607524,6.14831672291658));
#3844=CARTESIAN_POINT('Ctrl Pts',(-3.91604629967915,-25.1838353260752,6.26290005624954));
#3845=CARTESIAN_POINT('Ctrl Pts',(-3.53998077585005,-24.5578175514078,6.32019172291661));
#3846=CARTESIAN_POINT('Ctrl Pts',(-2.53317668706739,-23.5541511604319,6.43477505624951));
#3847=CARTESIAN_POINT('Ctrl Pts',(-1.90336339087076,-23.1775005077857,6.49206672291618));
#3848=CARTESIAN_POINT('Ctrl Pts',(-0.535707634461822,-22.7649451919414,
6.60665005624995));
#3849=CARTESIAN_POINT('Ctrl Pts',(0.200842052573385,-22.7294864032627,6.66394172291654));
#3850=CARTESIAN_POINT('Ctrl Pts',(1.60825741243838,-23.0117008784331,6.77852505624958));
#3851=CARTESIAN_POINT('Ctrl Pts',(2.27776629761871,-23.3291566705507,6.83581672291669));
#3852=CARTESIAN_POINT('Ctrl Pts',(3.39129936374918,-24.2458798314691,6.95040005624944));
#3853=CARTESIAN_POINT('Ctrl Pts',(3.8342243732566,-24.8443116308563,7.00769172291627));
#3854=CARTESIAN_POINT('Ctrl Pts',(4.38677541995195,-26.1840855712311,7.12227505624986));
#3855=CARTESIAN_POINT('Ctrl Pts',(4.49582343090945,-26.9241665562002,7.1795667229166));
#3856=CARTESIAN_POINT('Ctrl Pts',(4.35088796536903,-28.3730853248421,7.29415005624953));
#3857=CARTESIAN_POINT('Ctrl Pts',(4.09698986764256,-29.0805318136941,7.35144172291661));
#3858=CARTESIAN_POINT('Ctrl Pts',(3.28231577569086,-30.295784222617,7.46602505624951));
#3859=CARTESIAN_POINT('Ctrl Pts',(2.72227460111075,-30.8023978842609,7.52331672291659));
#3860=CARTESIAN_POINT('Ctrl Pts',(1.42483950789472,-31.4933756465881,7.63790005624954));
#3861=CARTESIAN_POINT('Ctrl Pts',(0.688661495622512,-31.6770315464534,7.69519172291528));
#3862=CARTESIAN_POINT('Ctrl Pts',(-0.788204900376376,-31.6748128590733,
7.80977505625085));
#3863=CARTESIAN_POINT('Ctrl Pts',(-1.52748050021878,-31.4888868687303,7.86706672291669));
#3864=CARTESIAN_POINT('Ctrl Pts',(-2.83500516546561,-30.7874846314674,7.98165005624943));
#3865=CARTESIAN_POINT('Ctrl Pts',(-3.40197820894101,-30.2726321471241,8.03894172291615));
#3866=CARTESIAN_POINT('Ctrl Pts',(-4.22831013251146,-29.0319454966501,8.15352505624997));
#3867=CARTESIAN_POINT('Ctrl Pts',(-4.48683403091752,-28.3072684458016,8.21081672291615));
#3868=CARTESIAN_POINT('Ctrl Pts',(-4.63141500694981,-26.8166774531803,8.32540005624997));
#3869=CARTESIAN_POINT('Ctrl Pts',(-4.51728050926608,-26.0521841784596,8.38269172291643));
#3870=CARTESIAN_POINT('Ctrl Pts',(-3.93948695283954,-24.6630648478093,8.49727505624969));
#3871=CARTESIAN_POINT('Ctrl Pts',(-3.47633116581651,-24.0397881200713,8.55456672291628));
#3872=CARTESIAN_POINT('Ctrl Pts',(-2.3065979072983,-23.082683034536,8.66915005624984));
#3873=CARTESIAN_POINT('Ctrl Pts',(-1.60110545776092,-22.7498116285361,8.72644172291626));
#3874=CARTESIAN_POINT('Ctrl Pts',(-0.1115431730045,-22.455781422157,8.84102505624986));
#3875=CARTESIAN_POINT('Ctrl Pts',(0.671112174616573,-22.4949563909962,8.89831672291601));
#3876=CARTESIAN_POINT('Ctrl Pts',(2.13000246784507,-22.9398244453587,9.01290005625012));
#3877=CARTESIAN_POINT('Ctrl Pts',(2.80482628686612,-23.3451431864166,9.07019172291636));
#3878=CARTESIAN_POINT('Ctrl Pts',(3.88662668511606,-24.4300812824538,9.18477505624977));
#3879=CARTESIAN_POINT('Ctrl Pts',(4.29253055496877,-25.1087006230277,9.24206672291584));
#3880=CARTESIAN_POINT('Ctrl Pts',(4.73716179724122,-26.5820965379602,9.35665005625028));
#3881=CARTESIAN_POINT('Ctrl Pts',(4.77541261016421,-27.3754791844964,9.41394172291549));
#3882=CARTESIAN_POINT('Ctrl Pts',(4.47164101091353,-28.8912695257086,9.52852505625063));
#3883=CARTESIAN_POINT('Ctrl Pts',(4.12985669269715,-29.6122167575113,9.58581672291576));
#3884=CARTESIAN_POINT('Ctrl Pts',(3.1430342330799,-30.8111660662582,9.70040005625036));
#3885=CARTESIAN_POINT('Ctrl Pts',(2.49889872045615,-31.2879872596437,9.75769172291579));
#3886=CARTESIAN_POINT('Ctrl Pts',(1.05703777990366,-31.8828241263658,9.87227505625033));
#3887=CARTESIAN_POINT('Ctrl Pts',(0.260671167899412,-32.0002213213825,9.92956672291638));
#3888=CARTESIAN_POINT('Ctrl Pts',(-1.29821369458701,-31.8444551409501,10.0441500562497));
#3889=CARTESIAN_POINT('Ctrl Pts',(-2.05923545291888,-31.5713875052691,10.1014417229165));
#3890=CARTESIAN_POINT('Ctrl Pts',(-3.36636373470387,-30.6953239177476,10.2160250562496));
#3891=CARTESIAN_POINT('Ctrl Pts',(-3.91119010810414,-30.0931215128015,10.2733167229167));
#3892=CARTESIAN_POINT('Ctrl Pts',(-4.65425634850692,-28.6982357313908,10.3879000562494));
#3893=CARTESIAN_POINT('Ctrl Pts',(-4.85173818484261,-27.906861497377,10.4451917229149));
#3894=CARTESIAN_POINT('Ctrl Pts',(-4.85062884134398,-27.1131792015253,10.5024833895831));
#3895=CARTESIAN_POINT('Ctrl Pts',(-4.49992531496781,-27.1253399927944,-0.498733179016745));
#3896=CARTESIAN_POINT('Ctrl Pts',(-4.50080577640339,-26.3890414230237,-0.441441512350059));
#3897=CARTESIAN_POINT('Ctrl Pts',(-4.31740187521755,-25.6514004960575,-0.38414984568344));
#3898=CARTESIAN_POINT('Ctrl Pts',(-3.62152187059884,-24.3457650353575,-0.26956651235005));
#3899=CARTESIAN_POINT('Ctrl Pts',(-3.10966424169642,-23.7790447241712,-0.212274845683405));
#3900=CARTESIAN_POINT('Ctrl Pts',(-1.87473833045347,-22.9517757677986,-0.0976915123500845));
#3901=CARTESIAN_POINT('Ctrl Pts',(-1.15282164350167,-22.6920629943005,-0.0403998456834014));
#3902=CARTESIAN_POINT('Ctrl Pts',(0.333130544922134,-22.5439400354353,0.0741834876499117));
#3903=CARTESIAN_POINT('Ctrl Pts',(1.09574982783323,-22.6557248123599,0.131475154316599));
#3904=CARTESIAN_POINT('Ctrl Pts',(2.48244777760786,-23.2282079016538,0.246058487649911));
#3905=CARTESIAN_POINT('Ctrl Pts',(3.10517944279315,-23.68840802634,0.30335015431662));
#3906=CARTESIAN_POINT('Ctrl Pts',(4.06265239793424,-24.85231643994,0.41793348764989));
#3907=CARTESIAN_POINT('Ctrl Pts',(4.3964363912496,-25.5549452872785,0.475225154316493));
#3908=CARTESIAN_POINT('Ctrl Pts',(4.69353684255108,-27.0395439300089,0.589808487650017));
#3909=CARTESIAN_POINT('Ctrl Pts',(4.65651659660415,-27.8201039966141,0.647100154316588));
#3910=CARTESIAN_POINT('Ctrl Pts',(4.21669610116961,-29.276064051845,0.761683487649922));
#3911=CARTESIAN_POINT('Ctrl Pts',(3.8142653646997,-29.950055727301,0.818975154316564));
#3912=CARTESIAN_POINT('Ctrl Pts',(2.73516012282014,-31.0316512891878,0.933558487649946));
#3913=CARTESIAN_POINT('Ctrl Pts',(2.05948004468961,-31.4381826698554,0.990850154316524));
#3914=CARTESIAN_POINT('Ctrl Pts',(0.591324807038797,-31.8853828510085,1.10543348764999));
#3915=CARTESIAN_POINT('Ctrl Pts',(-0.199761447971984,-31.9255726377888,
1.16272515431667));
#3916=CARTESIAN_POINT('Ctrl Pts',(-1.71214091388154,-31.6265370785213,1.27730848764984));
#3917=CARTESIAN_POINT('Ctrl Pts',(-2.43197693509141,-31.2875452940623,1.33460015431656));
#3918=CARTESIAN_POINT('Ctrl Pts',(-3.63015067419501,-30.306507524294,1.44918348764995));
#3919=CARTESIAN_POINT('Ctrl Pts',(-4.10730825861232,-29.6653586276362,1.50647515431652));
#3920=CARTESIAN_POINT('Ctrl Pts',(-4.70418801790555,-28.2289649290438,1.62105848764999));
#3921=CARTESIAN_POINT('Ctrl Pts',(-4.82328976434201,-27.4350737035586,1.67835015431658));
#3922=CARTESIAN_POINT('Ctrl Pts',(-4.67190249432477,-25.8800475050968,1.79293348764993));
#3923=CARTESIAN_POINT('Ctrl Pts',(-4.40150502792665,-25.1204053228213,1.85022515431664));
#3924=CARTESIAN_POINT('Ctrl Pts',(-3.53112225622387,-23.8146158747871,1.96480848764987));
#3925=CARTESIAN_POINT('Ctrl Pts',(-2.93192505802151,-23.2697474697807,2.02210015431647));
#3926=CARTESIAN_POINT('Ctrl Pts',(-1.54268043071708,-22.5251840572753,2.13668348765005));
#3927=CARTESIAN_POINT('Ctrl Pts',(-0.753936727410522,-22.3262485075428,
2.19397515431668));
#3928=CARTESIAN_POINT('Ctrl Pts',(0.82915854962663,-22.3244875853603,2.30855848764983));
#3929=CARTESIAN_POINT('Ctrl Pts',(1.62199572723047,-22.5217174227832,2.36585015431672));
#3930=CARTESIAN_POINT('Ctrl Pts',(3.02508187654173,-23.2696859056385,2.48043348764979));
#3931=CARTESIAN_POINT('Ctrl Pts',(3.63396341774869,-23.8197562460487,2.53772515431626));
#3932=CARTESIAN_POINT('Ctrl Pts',(4.52262186996503,-25.1465580304901,2.65230848765025));
#3933=CARTESIAN_POINT('Ctrl Pts',(4.80150418123824,-25.9220499865487,2.70960015431671));
#3934=CARTESIAN_POINT('Ctrl Pts',(4.96045785508009,-27.5179682692268,2.8241834876498));
#3935=CARTESIAN_POINT('Ctrl Pts',(4.84032389411636,-28.3368731787678,2.88147515431622));
#3936=CARTESIAN_POINT('Ctrl Pts',(4.22555498467076,-29.8256581291208,2.99605848765029));
#3937=CARTESIAN_POINT('Ctrl Pts',(3.7314586763185,-30.4940935072009,3.05335015431664));
#3938=CARTESIAN_POINT('Ctrl Pts',(2.48213401980284,-31.5216657613235,3.16793348764987));
#3939=CARTESIAN_POINT('Ctrl Pts',(1.72806682617598,-31.8797782805327,3.2252251543166));
#3940=CARTESIAN_POINT('Ctrl Pts',(0.13509320172947,-32.1984358560416,3.33980848764991));
#3941=CARTESIAN_POINT('Ctrl Pts',(-0.702299823999385,-32.1586235858217,
3.39710015431637));
#3942=CARTESIAN_POINT('Ctrl Pts',(-2.26400003813965,-31.6867271638891,3.51168348765014));
#3943=CARTESIAN_POINT('Ctrl Pts',(-2.98679775763238,-31.2550432103659,3.5689751543166));
#3944=CARTESIAN_POINT('Ctrl Pts',(-4.14652732706892,-30.0978039609755,3.68355848764991));
#3945=CARTESIAN_POINT('Ctrl Pts',(-4.58231192474403,-29.3733178387791,3.74085015431648));
#3946=CARTESIAN_POINT('Ctrl Pts',(-5.06158803244764,-27.7994224422382,3.85543348765003));
#3947=CARTESIAN_POINT('Ctrl Pts',(-5.10456984344478,-26.9515032280969,3.91272515431634));
#3948=CARTESIAN_POINT('Ctrl Pts',(-4.78397716002945,-25.3307487804658,4.02730848765017));
#3949=CARTESIAN_POINT('Ctrl Pts',(-4.42065684961388,-24.5594744129683,4.08460015431674));
#3950=CARTESIAN_POINT('Ctrl Pts',(-3.36951978092995,-23.275884430953,4.19918348764977));
#3951=CARTESIAN_POINT('Ctrl Pts',(-2.68266717130709,-22.764830662879,4.25647515431655));
#3952=CARTESIAN_POINT('Ctrl Pts',(-1.14418647221071,-22.1256650834116,4.37105848764996));
#3953=CARTESIAN_POINT('Ctrl Pts',(-0.294009620031413,-21.9982141529788,
4.42835015431673));
#3954=CARTESIAN_POINT('Ctrl Pts',(1.3709826726307,-22.1604321379097,4.54293348764978));
#3955=CARTESIAN_POINT('Ctrl Pts',(2.18420012405877,-22.4499991421574,4.60022515431661));
#3956=CARTESIAN_POINT('Ctrl Pts',(3.58186544525391,-23.3817714096182,4.7148084876499));
#3957=CARTESIAN_POINT('Ctrl Pts',(4.16494656178229,-24.0231298379359,4.77210015431648));
#3958=CARTESIAN_POINT('Ctrl Pts',(4.96159845253322,-25.5098251537481,4.88668348765003));
#3959=CARTESIAN_POINT('Ctrl Pts',(5.17435993882992,-26.3537650899519,4.94397515431683));
#3960=CARTESIAN_POINT('Ctrl Pts',(5.17612086103765,-28.0473585400691,5.05855848764968));
#3961=CARTESIAN_POINT('Ctrl Pts',(4.96506508699686,-28.8953919505567,5.11585015431639));
#3962=CARTESIAN_POINT('Ctrl Pts',(4.16500812595277,-30.3959287884026,5.23043348765012));
#3963=CARTESIAN_POINT('Ctrl Pts',(3.57672507396265,-31.0469715596972,5.28772515431631));
#3964=CARTESIAN_POINT('Ctrl Pts',(2.15804741641932,-31.9970195077,5.4023084876502));
#3965=CARTESIAN_POINT('Ctrl Pts',(1.32898019116406,-32.2950713567837,5.45960015431648));
#3966=CARTESIAN_POINT('Ctrl Pts',(-0.376904185685347,-32.4648557455888,
5.57418348765003));
#3967=CARTESIAN_POINT('Ctrl Pts',(-1.25209472194662,-32.3363726005772,5.63147515431663));
#3968=CARTESIAN_POINT('Ctrl Pts',(-2.84296667278025,-31.6793178710107,5.74605848764988));
#3969=CARTESIAN_POINT('Ctrl Pts',(-3.55710576383776,-31.1513253789313,5.80335015431639));
#3970=CARTESIAN_POINT('Ctrl Pts',(-4.65477731687436,-29.8165844795914,5.91793348765012));
#3971=CARTESIAN_POINT('Ctrl Pts',(-5.03721836201938,-29.0110789395971,5.97522515431631));
#3972=CARTESIAN_POINT('Ctrl Pts',(-5.37743306171915,-27.3097303335012,6.0898084876502));
#3973=CARTESIAN_POINT('Ctrl Pts',(-5.33482876722501,-26.4155043485724,6.14710015431696));
#3974=CARTESIAN_POINT('Ctrl Pts',(-4.83085641881337,-24.7480639756086,6.26168348764955));
#3975=CARTESIAN_POINT('Ctrl Pts',(-4.36991924819774,-23.9764602120055,6.31897515431661));
#3976=CARTESIAN_POINT('Ctrl Pts',(-3.13454599135584,-22.7385966350808,6.4335584876499));
#3977=CARTESIAN_POINT('Ctrl Pts',(-2.36125382501729,-22.2735588203518,6.49085015431656));
#3978=CARTESIAN_POINT('Ctrl Pts',(-0.681618269679574,-21.7622067861288,
6.60543348764995));
#3979=CARTESIAN_POINT('Ctrl Pts',(0.223133903687647,-21.7164329509015,6.66272515431674));
#3980=CARTESIAN_POINT('Ctrl Pts',(1.95226333294297,-22.0585827584601,6.77730848764977));
#3981=CARTESIAN_POINT('Ctrl Pts',(2.77497604680507,-22.4462315948605,6.83460015431688));
#3982=CARTESIAN_POINT('Ctrl Pts',(4.14398227167528,-23.5674679624083,6.94918348764963));
#3983=CARTESIAN_POINT('Ctrl Pts',(4.68893222344454,-24.3000242850548,7.00647515431646));
#3984=CARTESIAN_POINT('Ctrl Pts',(5.37038362306584,-25.9405919845896,7.12105848765005));
#3985=CARTESIAN_POINT('Ctrl Pts',(5.50618373750129,-26.8470544635367,7.17835015431679));
#3986=CARTESIAN_POINT('Ctrl Pts',(5.33313503766439,-28.6220128503173,7.29293348764972));
#3987=CARTESIAN_POINT('Ctrl Pts',(5.02439849553529,-29.4888055709765,7.3502251543168));
#3988=CARTESIAN_POINT('Ctrl Pts',(4.03123673237243,-30.9783467652573,7.46480848764971));
#3989=CARTESIAN_POINT('Ctrl Pts',(3.34771707388356,-31.5996405933702,7.52210015431658));
#3990=CARTESIAN_POINT('Ctrl Pts',(1.76357106961933,-32.4483809623168,7.63668348764993));
#3991=CARTESIAN_POINT('Ctrl Pts',(0.864434900460165,-32.6749683852002,7.69397515431566));
#3992=CARTESIAN_POINT('Ctrl Pts',(-0.939656722676682,-32.676729307438,7.80855848765085));
#3993=CARTESIAN_POINT('Ctrl Pts',(-1.84288636612563,-32.4518475967632,7.86585015431688));
#3994=CARTESIAN_POINT('Ctrl Pts',(-3.44087389241161,-31.5997021575577,7.98043348764962));
#3995=CARTESIAN_POINT('Ctrl Pts',(-4.13407789386612,-30.9732063939501,8.03772515431634));
#3996=CARTESIAN_POINT('Ctrl Pts',(-5.14551533760529,-29.4626528633526,8.15230848765016));
#3997=CARTESIAN_POINT('Ctrl Pts',(-5.46273672453315,-28.5800103688324,8.20960015431635));
#3998=CARTESIAN_POINT('Ctrl Pts',(-5.64335182828418,-26.7641598979005,8.32418348765016));
#3999=CARTESIAN_POINT('Ctrl Pts',(-5.50651949921481,-25.8326837348359,8.38147515431663));
#4000=CARTESIAN_POINT('Ctrl Pts',(-4.80717894956453,-24.139724783599,8.49605848764988));
#4001=CARTESIAN_POINT('Ctrl Pts',(-4.24529027372504,-23.379881979507,8.55335015431647));
#4002=CARTESIAN_POINT('Ctrl Pts',(-2.82513313158961,-22.2121111275932,8.66793348765004));
#4003=CARTESIAN_POINT('Ctrl Pts',(-1.96818924517237,-21.8053415564794,8.72522515431646));
#4004=CARTESIAN_POINT('Ctrl Pts',(-0.158465657509371,-21.4435697326178,
8.83980848765005));
#4005=CARTESIAN_POINT('Ctrl Pts',(0.792593286692538,-21.4889660513795,8.8971001543162));
#4006=CARTESIAN_POINT('Ctrl Pts',(2.56577381841575,-22.0250143262545,9.01168348765031));
#4007=CARTESIAN_POINT('Ctrl Pts',(3.38618362619219,-22.5152047139933,9.06897515431655));
#4008=CARTESIAN_POINT('Ctrl Pts',(4.70218121054346,-23.828711978241,9.18355848764996));
#4009=CARTESIAN_POINT('Ctrl Pts',(5.19647224236993,-24.6508101887781,9.24085015431603));
#4010=CARTESIAN_POINT('Ctrl Pts',(5.73990020308659,-26.4361859028455,9.35543348765047));
#4011=CARTESIAN_POINT('Ctrl Pts',(5.78846606254352,-27.3977710355077,9.41272515431568));
#4012=CARTESIAN_POINT('Ctrl Pts',(5.42475913086839,-29.2352754463162,9.52730848765082));
#4013=CARTESIAN_POINT('Ctrl Pts',(5.01278176845109,-30.1094265066166,9.58460015431595));
#4014=CARTESIAN_POINT('Ctrl Pts',(3.82144610207693,-31.5638489742655,9.69918348765055));
#4015=CARTESIAN_POINT('Ctrl Pts',(3.04318606635087,-32.1426951097914,9.75647515431598));
#4016=CARTESIAN_POINT('Ctrl Pts',(1.30053136645192,-32.86643232952,9.87105848765053));
#4017=CARTESIAN_POINT('Ctrl Pts',(0.337783260665778,-33.0105816279838,9.92835015431657));
#4018=CARTESIAN_POINT('Ctrl Pts',(-1.54714122016509,-32.826702213236,10.0429334876499));
#4019=CARTESIAN_POINT('Ctrl Pts',(-2.4675092101147,-32.4987961332167,10.1002251543167));
#4020=CARTESIAN_POINT('Ctrl Pts',(-4.04892627743074,-31.4442448743743,10.2148084876498));
#4021=CARTESIAN_POINT('Ctrl Pts',(-4.70843281716765,-30.7185639856579,10.2721001543169));
#4022=CARTESIAN_POINT('Ctrl Pts',(-5.60926166428151,-29.0369672930318,10.3866834876496));
#4023=CARTESIAN_POINT('Ctrl Pts',(-5.84967502356038,-28.082634904679,10.4439751543151));
#4024=CARTESIAN_POINT('Ctrl Pts',(-5.85055548489976,-27.125339992794,10.5012668209833));
#4025=CARTESIAN_POINT('Ctrl Pts',(-4.49992531496781,-27.2248833652324,0.496300045053516));
#4026=CARTESIAN_POINT('Ctrl Pts',(-4.5170935228935,-26.4885847954605,0.553591711720202));
#4027=CARTESIAN_POINT('Ctrl Pts',(-4.34996178652419,-25.7468679032987,0.610883378386821));
#4028=CARTESIAN_POINT('Ctrl Pts',(-3.68281080117209,-24.4258764618724,0.725466711720211));
#4029=CARTESIAN_POINT('Ctrl Pts',(-3.18338254408968,-23.8478908247253,0.782758378386896));
#4030=CARTESIAN_POINT('Ctrl Pts',(-1.96655460663691,-22.9935363364864,0.897341711720136));
#4031=CARTESIAN_POINT('Ctrl Pts',(-1.25028920909816,-22.7180292671551,0.954633378386819));
#4032=CARTESIAN_POINT('Ctrl Pts',(0.232470022735047,-22.537487675991,1.06921671172021));
#4033=CARTESIAN_POINT('Ctrl Pts',(0.997550692859376,-22.6326791281778,1.12650837838686));
#4034=CARTESIAN_POINT('Ctrl Pts',(2.39671474379638,-23.1750663869683,1.24109171172017));
#4035=CARTESIAN_POINT('Ctrl Pts',(3.02943919783654,-23.6217927956222,1.29838337838692));
#4036=CARTESIAN_POINT('Ctrl Pts',(4.01209334897545,-24.7650355357426,1.41296671172011));
#4037=CARTESIAN_POINT('Ctrl Pts',(4.36104166103753,-25.4604921944619,1.47025837838671));
#4038=CARTESIAN_POINT('Ctrl Pts',(4.69009167559614,-26.9387356739276,1.58484171172032));
#4039=CARTESIAN_POINT('Ctrl Pts',(4.66982611111995,-27.7201188452534,1.64213337838685));
#4040=CARTESIAN_POINT('Ctrl Pts',(4.26117841813581,-29.1855350667241,1.75671671172018));
#4041=CARTESIAN_POINT('Ctrl Pts',(3.87313598265158,-29.8681507579074,1.81400837838683));
#4042=CARTESIAN_POINT('Ctrl Pts',(2.8170650922145,-30.9727806712352,1.92859171172021));
#4043=CARTESIAN_POINT('Ctrl Pts',(2.15000902980881,-31.3937003528865,1.98588337838683));
#4044=CARTESIAN_POINT('Ctrl Pts',(0.691309958401167,-31.8720733364954,2.10046671172021));
#4045=CARTESIAN_POINT('Ctrl Pts',(-0.0989531918895839,-31.929017804739,
2.15775837838676));
#4046=CARTESIAN_POINT('Ctrl Pts',(-1.61768782106606,-31.6619318087381,2.27234171172027));
#4047=CARTESIAN_POINT('Ctrl Pts',(-2.34469603088869,-31.3381043430165,2.32963337838682));
#4048=CARTESIAN_POINT('Ctrl Pts',(-3.56353544348255,-30.3822477692553,2.44421671172021));
#4049=CARTESIAN_POINT('Ctrl Pts',(-4.05416674391711,-29.751091661441,2.50150837838678));
#4050=CARTESIAN_POINT('Ctrl Pts',(-4.68114233373318,-28.3271640640242,2.61609171172026));
#4051=CARTESIAN_POINT('Ctrl Pts',(-4.81683740488648,-27.535734225746,2.67338337838684));
#4052=CARTESIAN_POINT('Ctrl Pts',(-4.69786876719058,-25.977515070693,2.78796671172019));
#4053=CARTESIAN_POINT('Ctrl Pts',(-4.44326559660206,-25.2122215990087,2.8452583783869));
#4054=CARTESIAN_POINT('Ctrl Pts',(-3.59996835679039,-23.8883341771763,2.95984171172013));
#4055=CARTESIAN_POINT('Ctrl Pts',(-3.01203648453192,-23.3310364003662,3.01713337838681));
#4056=CARTESIAN_POINT('Ctrl Pts',(-1.6381478379628,-22.5577439685697,3.13171671172022));
#4057=CARTESIAN_POINT('Ctrl Pts',(-0.853480099848572,-22.3425362536569,
3.18900837838685));
#4058=CARTESIAN_POINT('Ctrl Pts',(0.729615177188581,-22.3081998392462,3.30359171172018));
#4059=CARTESIAN_POINT('Ctrl Pts',(1.5265283199834,-22.4891575114895,3.36088337838689));
#4060=CARTESIAN_POINT('Ctrl Pts',(2.94497045003267,-23.2083969750522,3.47546671172014));
#4061=CARTESIAN_POINT('Ctrl Pts',(3.56511731717984,-23.7460379436645,3.53275837838669));
#4062=CARTESIAN_POINT('Ctrl Pts',(4.48086130129196,-25.0547417542976,3.64734171172034));
#4063=CARTESIAN_POINT('Ctrl Pts',(4.77553790836679,-25.8245824209521,3.70463337838689));
#4064=CARTESIAN_POINT('Ctrl Pts',(4.96691021454127,-27.4173077470399,3.81921671172015));
#4065=CARTESIAN_POINT('Ctrl Pts',(4.86336957828356,-28.2386740437859,3.87650837838657));
#4066=CARTESIAN_POINT('Ctrl Pts',(4.27869649937114,-29.7399250953174,3.99109171172046));
#4067=CARTESIAN_POINT('Ctrl Pts',(3.7980739070243,-30.4183532622312,4.0483833783869));
#4068=CARTESIAN_POINT('Ctrl Pts',(2.56941492401223,-31.4711067123778,4.16296671172013));
#4069=CARTESIAN_POINT('Ctrl Pts',(1.82251991899126,-31.8443835503049,4.22025837838686));
#4070=CARTESIAN_POINT('Ctrl Pts',(0.235901457812061,-32.1949906891023,4.33484171172017));
#4071=CARTESIAN_POINT('Ctrl Pts',(-0.602314672632131,-32.1719331003238,
4.39213337838664));
#4072=CARTESIAN_POINT('Ctrl Pts',(-2.17347105302534,-31.731209480869,4.5067167117204));
#4073=CARTESIAN_POINT('Ctrl Pts',(-2.90489278822714,-31.3139138283048,4.56400837838686));
#4074=CARTESIAN_POINT('Ctrl Pts',(-4.0876567091279,-30.1797089303828,4.67859171172017));
#4075=CARTESIAN_POINT('Ctrl Pts',(-4.5378296077608,-29.4638468238943,4.73588337838674));
#4076=CARTESIAN_POINT('Ctrl Pts',(-5.04827851794888,-27.8994075936046,4.85046671172029));
#4077=CARTESIAN_POINT('Ctrl Pts',(-5.10801501038022,-27.0523114841814,4.9077583783866));
#4078=CARTESIAN_POINT('Ctrl Pts',(-4.81937189026103,-25.4252018732791,5.02234171172043));
#4079=CARTESIAN_POINT('Ctrl Pts',(-4.47121589855777,-24.6467553171812,5.07963337838682));
#4080=CARTESIAN_POINT('Ctrl Pts',(-3.44526002590146,-23.3424996616552,5.19421671172021));
#4081=CARTESIAN_POINT('Ctrl Pts',(-2.76840020510825,-22.8179721775895,5.25150837838681));
#4082=CARTESIAN_POINT('Ctrl Pts',(-1.24238560719488,-22.1487107675687,5.36609171172022));
#4083=CARTESIAN_POINT('Ctrl Pts',(-0.394670142221978,-22.0046665124503,
5.42338337838681));
#4084=CARTESIAN_POINT('Ctrl Pts',(1.27351510703769,-22.1344658650278,5.53796671172023));
#4085=CARTESIAN_POINT('Ctrl Pts',(2.09238384786002,-22.4082385734949,5.59525837838687));
#4086=CARTESIAN_POINT('Ctrl Pts',(3.50814714287596,-23.3129253090387,5.70984171172016));
#4087=CARTESIAN_POINT('Ctrl Pts',(4.10365763118507,-23.9430184114309,5.76713337838693));
#4088=CARTESIAN_POINT('Ctrl Pts',(4.92903854125055,-25.4143577464969,5.8817167117201));
#4089=CARTESIAN_POINT('Ctrl Pts',(5.15807219270217,-26.2542217175139,5.93900837838691));
#4090=CARTESIAN_POINT('Ctrl Pts',(5.1924086071654,-27.947815167631,6.05359171172013));
#4091=CARTESIAN_POINT('Ctrl Pts',(4.99762499827922,-28.7999245433053,6.11088337838665));
#4092=CARTESIAN_POINT('Ctrl Pts',(4.22629705655031,-30.315817361898,6.22546671172039));
#4093=CARTESIAN_POINT('Ctrl Pts',(3.65044337633885,-30.978125459117,6.28275837838657));
#4094=CARTESIAN_POINT('Ctrl Pts',(2.24986369261982,-31.9552589390383,6.39734171172046));
#4095=CARTESIAN_POINT('Ctrl Pts',(1.42644775675681,-32.2691050839008,6.45463337838693));
#4096=CARTESIAN_POINT('Ctrl Pts',(-0.276243663494525,-32.4713081050615,
6.56921671172011));
#4097=CARTESIAN_POINT('Ctrl Pts',(-1.1538955869619,-32.3594182847329,6.6265083783867));
#4098=CARTESIAN_POINT('Ctrl Pts',(-2.75723363897965,-31.7324593857226,6.74109171172033));
#4099=CARTESIAN_POINT('Ctrl Pts',(-3.48136551885855,-31.2179406096298,6.79838337838684));
#4100=CARTESIAN_POINT('Ctrl Pts',(-4.60421826793817,-29.9038653838081,6.91296671172019));
#4101=CARTESIAN_POINT('Ctrl Pts',(-5.00182363177902,-29.1055320324077,6.97025837838657));
#4102=CARTESIAN_POINT('Ctrl Pts',(-5.37398789479249,-27.4105385895884,7.08484171172046));
#4103=CARTESIAN_POINT('Ctrl Pts',(-5.34813828171182,-26.5154894999401,7.14213337838704));
#4104=CARTESIAN_POINT('Ctrl Pts',(-4.87533873580858,-24.8385929607225,7.25671671172));
#4105=CARTESIAN_POINT('Ctrl Pts',(-4.42878986612819,-24.0583651814228,7.31400837838707));
#4106=CARTESIAN_POINT('Ctrl Pts',(-3.21645096077164,-22.7974672530097,7.42859171171997));
#4107=CARTESIAN_POINT('Ctrl Pts',(-2.45178281012867,-22.3180411373462,7.48588337838663));
#4108=CARTESIAN_POINT('Ctrl Pts',(-0.781603421049769,-21.7755163006163,
7.6004667117204));
#4109=CARTESIAN_POINT('Ctrl Pts',(0.12232564759955,-21.7129877839796,7.657758378387));
#4110=CARTESIAN_POINT('Ctrl Pts',(1.85781024013319,-22.023188028215,7.77234171172004));
#4111=CARTESIAN_POINT('Ctrl Pts',(2.68769514258573,-22.3956725459287,7.82963337838637));
#4112=CARTESIAN_POINT('Ctrl Pts',(4.07736704097944,-23.4917277174247,7.94421671172066));
#4113=CARTESIAN_POINT('Ctrl Pts',(4.6357907087237,-24.2142912512598,8.00150837838672));
#4114=CARTESIAN_POINT('Ctrl Pts',(5.34733793891911,-25.8423928495992,8.11609171172032));
#4115=CARTESIAN_POINT('Ctrl Pts',(5.4997313780195,-26.746393941348,8.17338337838705));
#4116=CARTESIAN_POINT('Ctrl Pts',(5.35910131055647,-28.5245452847223,8.28796671171998));
#4117=CARTESIAN_POINT('Ctrl Pts',(5.06615906418831,-29.3969892947731,8.34525837838706));
#4118=CARTESIAN_POINT('Ctrl Pts',(4.10008283296135,-30.904628462884,8.45984171171997));
#4119=CARTESIAN_POINT('Ctrl Pts',(3.42782850038057,-31.5383516627646,8.51713337838782));
#4120=CARTESIAN_POINT('Ctrl Pts',(1.85903847687845,-32.4158210510425,8.63171671171921));
#4121=CARTESIAN_POINT('Ctrl Pts',(0.963978272898216,-32.6586806390649,8.68900837838573));
#4122=CARTESIAN_POINT('Ctrl Pts',(-0.840113350238634,-32.6930170535733,
8.80359171172131));
#4123=CARTESIAN_POINT('Ctrl Pts',(-1.74741895886588,-32.4844075080322,8.86088337838715));
#4124=CARTESIAN_POINT('Ctrl Pts',(-3.36076246591524,-31.6609910881686,8.97546671171988));
#4125=CARTESIAN_POINT('Ctrl Pts',(-4.06523179327696,-31.0469246963195,9.03275837838661));
#4126=CARTESIAN_POINT('Ctrl Pts',(-5.10375476895253,-29.5544691395598,9.14734171172043));
#4127=CARTESIAN_POINT('Ctrl Pts',(-5.43677045163593,-28.6774779344237,9.20463337838661));
#4128=CARTESIAN_POINT('Ctrl Pts',(-5.64980418777113,-26.8648204200928,9.31921671172042));
#4129=CARTESIAN_POINT('Ctrl Pts',(-5.5295651833589,-25.9308828698286,9.37650837838689));
#4130=CARTESIAN_POINT('Ctrl Pts',(-4.86032046428803,-24.2254578173917,9.49109171172014));
#4131=CARTESIAN_POINT('Ctrl Pts',(-4.3119055044145,-23.4556222244942,9.54838337838673));
#4132=CARTESIAN_POINT('Ctrl Pts',(-2.91241403581534,-22.2626701765213,9.6629667117203));
#4133=CARTESIAN_POINT('Ctrl Pts',(-2.06264233798167,-21.8407362867315,9.72025837838672));
#4134=CARTESIAN_POINT('Ctrl Pts',(-0.259273913597949,-21.4470148995327,
9.83484171172031));
#4135=CARTESIAN_POINT('Ctrl Pts',(0.692608135318521,-21.4756565369004,9.89213337838646));
#4136=CARTESIAN_POINT('Ctrl Pts',(2.47524483330821,-21.9805320092516,10.0067167117206));
#4137=CARTESIAN_POINT('Ctrl Pts',(3.30427865677026,-22.456334096069,10.0640083783868));
#4138=CARTESIAN_POINT('Ctrl Pts',(4.64331059261914,-23.746807008819,10.1785917117202));
#4139=CARTESIAN_POINT('Ctrl Pts',(5.15198992536476,-24.5602812036706,10.2358833783863));
#4140=CARTESIAN_POINT('Ctrl Pts',(5.72659068860977,-26.3362007514714,10.3504667117207));
#4141=CARTESIAN_POINT('Ctrl Pts',(5.79191122945707,-27.2969627794171,10.4077583783851));
#4142=CARTESIAN_POINT('Ctrl Pts',(5.46015386112188,-29.1408223535089,10.5223417117219));
#4143=CARTESIAN_POINT('Ctrl Pts',(5.0633408173762,-30.0221456023925,10.5796333783862));
#4144=CARTESIAN_POINT('Ctrl Pts',(3.89718634706722,-31.4972337435744,10.6942167117208));
#4145=CARTESIAN_POINT('Ctrl Pts',(3.12891910014267,-32.0895535950602,10.7515083783862));
#4146=CARTESIAN_POINT('Ctrl Pts',(1.39873050144544,-32.8433866453836,10.8660917117208));
#4147=CARTESIAN_POINT('Ctrl Pts',(0.438443782857998,-33.004129268492,10.9233833783868));
#4148=CARTESIAN_POINT('Ctrl Pts',(-1.44967365457374,-32.8526684861381,11.0379667117202));
#4149=CARTESIAN_POINT('Ctrl Pts',(-2.37569293390397,-32.5405567018643,11.095258378387));
#4150=CARTESIAN_POINT('Ctrl Pts',(-3.97520797506477,-31.5130909749686,11.2098417117201));
#4151=CARTESIAN_POINT('Ctrl Pts',(-4.64714388655123,-30.7986754121516,11.2671333783872));
#4152=CARTESIAN_POINT('Ctrl Pts',(-5.57670175301804,-29.1324347002942,11.3817167117199));
#4153=CARTESIAN_POINT('Ctrl Pts',(-5.83338727717491,-28.1821782771171,11.4390083783853));
#4154=CARTESIAN_POINT('Ctrl Pts',(-5.85055548489977,-27.224883365232,11.4963000450535));
#4155=CARTESIAN_POINT('Ctrl Pts',(-3.5,-27.2127225901214,0.49751661203513));
#4156=CARTESIAN_POINT('Ctrl Pts',(-3.51517840571961,-26.6400364200585,0.554808278701816));
#4157=CARTESIAN_POINT('Ctrl Pts',(-3.3870023381626,-26.0622733505102,0.612099945368435));
#4158=CARTESIAN_POINT('Ctrl Pts',(-2.87059435406378,-25.0317443834292,0.726683278701825));
#4159=CARTESIAN_POINT('Ctrl Pts',(-2.48280922845853,-24.5799895371609,0.78397494536851));
#4160=CARTESIAN_POINT('Ctrl Pts',(-1.5358478118566,-23.9107403226621,0.89855827870175));
#4161=CARTESIAN_POINT('Ctrl Pts',(-0.9775476488716,-23.6939306641498,0.955849945368433));
#4162=CARTESIAN_POINT('Ctrl Pts',(0.179952537651027,-23.5494231527329,1.07043327870183));
#4163=CARTESIAN_POINT('Ctrl Pts',(0.778050540497913,-23.6219168035854,1.12772494536847));
#4164=CARTESIAN_POINT('Ctrl Pts',(1.8733753753257,-24.0427572309574,1.24230827870179));
#4165=CARTESIAN_POINT('Ctrl Pts',(2.36953393381726,-24.3907508815125,1.29959994536854));
#4166=CARTESIAN_POINT('Ctrl Pts',(3.14152259901176,-25.2835700713775,1.41418327870172));
#4167=CARTESIAN_POINT('Ctrl Pts',(3.41657284380058,-25.8275754937386,1.47147494536833));
#4168=CARTESIAN_POINT('Ctrl Pts',(3.67788133105185,-26.9856580964836,1.58605827870193));
#4169=CARTESIAN_POINT('Ctrl Pts',(3.6638371082595,-27.5986378942041,1.64334994536846));
#4170=CARTESIAN_POINT('Ctrl Pts',(3.34636951441486,-28.7497642955404,1.7579332787018));
#4171=CARTESIAN_POINT('Ctrl Pts',(3.04319861323196,-29.2867941907393,1.81522494536844));
#4172=CARTESIAN_POINT('Ctrl Pts',(2.21569658675549,-30.1572272297066,1.92980827870182));
#4173=CARTESIAN_POINT('Ctrl Pts',(1.69211920432461,-30.4897598664222,1.98709994536844));
#4174=CARTESIAN_POINT('Ctrl Pts',(0.545399516782365,-30.8693362630914,2.10168327870182));
#4175=CARTESIAN_POINT('Ctrl Pts',(-0.0766613701186401,-30.9159656984605,
2.15897494536837));
#4176=CARTESIAN_POINT('Ctrl Pts',(-1.27368235791308,-30.7088149551059,2.27355827870189));
#4177=CARTESIAN_POINT('Ctrl Pts',(-1.84748694212142,-30.4551804406305,2.33084994536843));
#4178=CARTESIAN_POINT('Ctrl Pts',(-2.81085353585185,-29.7038368014157,2.44543327870183));
#4179=CARTESIAN_POINT('Ctrl Pts',(-3.19946002926004,-29.2068050390794,2.50272494536839));
#4180=CARTESIAN_POINT('Ctrl Pts',(-3.69753543763233,-28.0836708006555,2.61730827870187));
#4181=CARTESIAN_POINT('Ctrl Pts',(-3.80647844076847,-27.458622235808,2.67459994536846));
#4182=CARTESIAN_POINT('Ctrl Pts',(-3.71562299996974,-26.2264422651536,2.7891832787018));
#4183=CARTESIAN_POINT('Ctrl Pts',(-3.51585820108909,-25.6204948140464,2.84647494536852));
#4184=CARTESIAN_POINT('Ctrl Pts',(-2.85104839504354,-24.5708958126827,2.96105827870174));
#4185=CARTESIAN_POINT('Ctrl Pts',(-2.38659484300895,-24.1282780503191,3.01834994536843));
#4186=CARTESIAN_POINT('Ctrl Pts',(-1.29941672607197,-23.5127480152682,3.13293327870183));
#4187=CARTESIAN_POINT('Ctrl Pts',(-0.677706928819807,-23.3404717664636,
3.19022494536847));
#4188=CARTESIAN_POINT('Ctrl Pts',(0.578163556381843,-23.3101149563751,3.30480827870179));
#4189=CARTESIAN_POINT('Ctrl Pts',(1.2111228729238,-23.4521169599317,3.3620999453685));
#4190=CARTESIAN_POINT('Ctrl Pts',(2.33910252832393,-24.02061342208,3.47668327870176));
#4191=CARTESIAN_POINT('Ctrl Pts',(2.83301860484105,-24.4466112594378,3.53397494536822));
#4192=CARTESIAN_POINT('Ctrl Pts',(3.56365731501942,-25.4854485489357,3.64855827870204));
#4193=CARTESIAN_POINT('Ctrl Pts',(3.79963651139122,-26.0973239813465,3.70584994536859));
#4194=CARTESIAN_POINT('Ctrl Pts',(3.95497473778028,-27.364790261788,3.82043327870167));
#4195=CARTESIAN_POINT('Ctrl Pts',(3.87413190281369,-28.0191738915788,3.87772494536818));
#4196=CARTESIAN_POINT('Ctrl Pts',(3.41100565544429,-29.2165857266924,3.99230827870208));
#4197=CARTESIAN_POINT('Ctrl Pts',(3.02911582100773,-29.7584479983173,4.04959994536851));
#4198=CARTESIAN_POINT('Ctrl Pts',(2.05088038850359,-30.6005359623087,4.16418327870175));
#4199=CARTESIAN_POINT('Ctrl Pts',(1.45543661955604,-30.8999147331016,4.22147494536847));
#4200=CARTESIAN_POINT('Ctrl Pts',(0.188979035414647,-31.1827803445244,4.33605827870178));
#4201=CARTESIAN_POINT('Ctrl Pts',(-0.480833721736332,-31.1659440974169,
4.39334994536825));
#4202=CARTESIAN_POINT('Ctrl Pts',(-1.73770028168812,-30.8164005771944,4.50793327870201));
#4203=CARTESIAN_POINT('Ctrl Pts',(-2.32353622117369,-30.4839764587754,4.56522494536848));
#4204=CARTESIAN_POINT('Ctrl Pts',(-3.27210326748465,-29.5783404250336,4.67980827870178));
#4205=CARTESIAN_POINT('Ctrl Pts',(-3.63388912134312,-29.0059569982611,4.73709994536835));
#4206=CARTESIAN_POINT('Ctrl Pts',(-4.04554144449821,-27.7534971521348,4.85168327870191));
#4207=CARTESIAN_POINT('Ctrl Pts',(-4.09496290407286,-27.0746033058008,4.90897494536821));
#4208=CARTESIAN_POINT('Ctrl Pts',(-3.86625503665767,-25.7692073365837,5.02355827870204));
#4209=CARTESIAN_POINT('Ctrl Pts',(-3.58829199607698,-25.1439644058301,5.08084994536843));
#4210=CARTESIAN_POINT('Ctrl Pts',(-2.76684905815666,-24.0951815694044,5.19543327870183));
#4211=CARTESIAN_POINT('Ctrl Pts',(-2.22411358260874,-23.6726788921877,5.25272494536842));
#4212=CARTESIAN_POINT('Ctrl Pts',(-0.998892343964084,-23.1323176637283,
5.36730827870184));
#4213=CARTESIAN_POINT('Ctrl Pts',(-0.317558152137087,-23.0150254765812,
5.42459994536842));
#4214=CARTESIAN_POINT('Ctrl Pts',(1.02458791243016,-23.1167116322358,5.53918327870184));
#4215=CARTESIAN_POINT('Ctrl Pts',(1.68411063294507,-23.3356459690878,5.59647494536849));
#4216=CARTESIAN_POINT('Ctrl Pts',(2.82558550724685,-24.0618452707057,5.71105827870177));
#4217=CARTESIAN_POINT('Ctrl Pts',(3.30641598130079,-24.5684600530816,5.76834994536854));
#4218=CARTESIAN_POINT('Ctrl Pts',(3.97403449448334,-25.75308885826,5.88293327870172));
#4219=CARTESIAN_POINT('Ctrl Pts',(4.16013667989657,-26.4299948886844,5.94022494536852));
#4220=CARTESIAN_POINT('Ctrl Pts',(4.19049349003537,-27.7963635466824,6.05480827870174));
#4221=CARTESIAN_POINT('Ctrl Pts',(4.03466554977154,-28.4845190963707,6.11209994536826));
#4222=CARTESIAN_POINT('Ctrl Pts',(3.41408060958811,-29.7099494400641,6.226683278702));
#4223=CARTESIAN_POINT('Ctrl Pts',(2.94987006045165,-30.2460267468577,6.28397494536819));
#4224=CARTESIAN_POINT('Ctrl Pts',(1.81915689809562,-31.0380549526863,6.39855827870207));
#4225=CARTESIAN_POINT('Ctrl Pts',(1.15370619622606,-31.2932036869398,6.45584994536854));
#4226=CARTESIAN_POINT('Ctrl Pts',(-0.223726178106239,-31.4593726282858,
6.57043327870172));
#4227=CARTESIAN_POINT('Ctrl Pts',(-0.934395434881124,-31.3701806092125,
6.62772494536832));
#4228=CARTESIAN_POINT('Ctrl Pts',(-2.2338942702282,-30.8647685418463,6.74230827870194));
#4229=CARTESIAN_POINT('Ctrl Pts',(-2.82146025502993,-30.4489825235109,6.79959994536845));
#4230=CARTESIAN_POINT('Ctrl Pts',(-3.73364751778378,-29.3853308484018,6.91418327870181));
#4231=CARTESIAN_POINT('Ctrl Pts',(-4.05735481460304,-28.7384487328433,6.97147494536818));
#4232=CARTESIAN_POINT('Ctrl Pts',(-4.36177755018722,-27.3636161673202,7.08605827870208));
#4233=CARTESIAN_POINT('Ctrl Pts',(-4.34214927877062,-26.6369704507106,7.14334994536865));
#4234=CARTESIAN_POINT('Ctrl Pts',(-3.96052983216839,-25.2743637321851,7.25793327870161));
#4235=CARTESIAN_POINT('Ctrl Pts',(-3.59885249650756,-24.6397217483839,7.31522494536868));
#4236=CARTESIAN_POINT('Ctrl Pts',(-2.61508245551368,-23.6130206947453,7.42980827870158));
#4237=CARTESIAN_POINT('Ctrl Pts',(-1.99389298437356,-23.2219816237259,7.48709994536824));
#4238=CARTESIAN_POINT('Ctrl Pts',(-0.635692979701946,-22.778253374105,7.60168327870201));
#4239=CARTESIAN_POINT('Ctrl Pts',(0.10003382610432,-22.7260398903107,7.65897494536861));
#4240=CARTESIAN_POINT('Ctrl Pts',(1.51380477670442,-22.9763048817946,7.77355827870165));
#4241=CARTESIAN_POINT('Ctrl Pts',(2.19048605403487,-23.2785964484885,7.83084994536837));
#4242=CARTESIAN_POINT('Ctrl Pts',(3.32468513313227,-24.1701386850904,7.94543327870189));
#4243=CARTESIAN_POINT('Ctrl Pts',(3.78108399417411,-24.758577873874,8.00272494536833));
#4244=CARTESIAN_POINT('Ctrl Pts',(4.36373104271076,-26.0858861127153,8.11730827870193));
#4245=CARTESIAN_POINT('Ctrl Pts',(4.48937241387869,-26.8235059315532,8.17459994536905));
#4246=CARTESIAN_POINT('Ctrl Pts',(4.37685554335844,-28.2756180899945,8.28918327870121));
#4247=CARTESIAN_POINT('Ctrl Pts',(4.13875166853063,-28.9887160799575,8.34647494536867));
#4248=CARTESIAN_POINT('Ctrl Pts',(3.35116287135924,-30.2220668271555,8.46105827870158));
#4249=CARTESIAN_POINT('Ctrl Pts',(2.80238685862471,-30.741110012937,8.51834994536944));
#4250=CARTESIAN_POINT('Ctrl Pts',(1.52030736522058,-31.4608170042187,8.63293327870083));
#4251=CARTESIAN_POINT('Ctrl Pts',(0.788205101607952,-31.6607451262615,8.69022494536734));
#4252=CARTESIAN_POINT('Ctrl Pts',(-0.688661729170329,-31.6911019364411,
8.80480827870292));
#4253=CARTESIAN_POINT('Ctrl Pts',(-1.43201351203358,-31.521448059472,8.86209994536876));
#4254=CARTESIAN_POINT('Ctrl Pts',(-2.75489454397912,-30.848774641259,8.9766832787015));
#4255=CARTESIAN_POINT('Ctrl Pts',(-3.33313308108255,-30.3463513803362,9.03397494536822));
#4256=CARTESIAN_POINT('Ctrl Pts',(-4.18655078253556,-29.1237623451318,9.14855827870204));
#4257=CARTESIAN_POINT('Ctrl Pts',(-4.46086905468824,-28.404736373781,9.20584994536822));
#4258=CARTESIAN_POINT('Ctrl Pts',(-4.63786871098225,-26.9173379055931,9.32043327870204));
#4259=CARTESIAN_POINT('Ctrl Pts',(-4.54032750779717,-26.1503830218042,9.3777249453685));
#4260=CARTESIAN_POINT('Ctrl Pts',(-3.99262962045306,-24.7487971862483,9.49230827870176));
#4261=CARTESIAN_POINT('Ctrl Pts',(-3.54294741821142,-24.1155274882508,9.54959994536835));
#4262=CARTESIAN_POINT('Ctrl Pts',(-2.39387950049328,-23.1332409267478,9.66418327870191));
#4263=CARTESIAN_POINT('Ctrl Pts',(-1.69555903830893,-22.7852051038846,9.72147494536834));
#4264=CARTESIAN_POINT('Ctrl Pts',(-0.212351491438122,-22.4592252441609,
9.83605827870193));
#4265=CARTESIAN_POINT('Ctrl Pts',(0.571127184652916,-22.4816455398733,9.89334994536808));
#4266=CARTESIAN_POINT('Ctrl Pts',(2.03947406174072,-22.8953409128601,10.0079332787022));
#4267=CARTESIAN_POINT('Ctrl Pts',(2.72292208988536,-23.2862714657652,10.0652249453684));
#4268=CARTESIAN_POINT('Ctrl Pts',(3.82775715080726,-24.3481755140014,10.1798082787018));
#4269=CARTESIAN_POINT('Ctrl Pts',(4.24804943901783,-25.0181710295281,10.2370999453679));
#4270=CARTESIAN_POINT('Ctrl Pts',(4.72385361508833,-26.4821111927169,10.3516832787023));
#4271=CARTESIAN_POINT('Ctrl Pts',(4.7788591231067,-27.2746709580248,10.4089749453667));
#4272=CARTESIAN_POINT('Ctrl Pts',(4.50703700756152,-28.7968168899771,10.5235582787035));
#4273=CARTESIAN_POINT('Ctrl Pts',(4.18041691475187,-29.5249365139219,10.5808499453678));
#4274=CARTESIAN_POINT('Ctrl Pts',(3.21877537946603,-30.7445518356469,10.6954332787024));
#4275=CARTESIAN_POINT('Ctrl Pts',(2.58463247743365,-31.2348468805496,10.7527249453679));
#4276=CARTESIAN_POINT('Ctrl Pts',(1.15523723842422,-31.8597797491362,10.8673082787024));
#4277=CARTESIAN_POINT('Ctrl Pts',(0.361331792548347,-31.9937703043426,10.9245999453685));
#4278=CARTESIAN_POINT('Ctrl Pts',(-1.20074645974137,-31.8704227189487,11.0391832787018));
#4279=CARTESIAN_POINT('Ctrl Pts',(-1.96741971917488,-31.6131493061509,11.0964749453686));
#4280=CARTESIAN_POINT('Ctrl Pts',(-3.29264633924976,-30.7641710134222,11.2110582787017));
#4281=CARTESIAN_POINT('Ctrl Pts',(-3.84990223677302,-30.1732337703105,11.2683499453688));
#4282=CARTESIAN_POINT('Ctrl Pts',(-4.62169770614474,-28.7937035887216,11.3829332787015));
#4283=CARTESIAN_POINT('Ctrl Pts',(-4.83545176440121,-28.0064051033624,11.440224945367));
#4284=CARTESIAN_POINT('Ctrl Pts',(-4.85063016993195,-27.212722590121,11.4975166120351));
#4285=CARTESIAN_POINT('Ctrl Pts',(-2.50007867078019,-27.2005618634838,0.498733174167452));
#4286=CARTESIAN_POINT('Ctrl Pts',(-2.51326728222517,-26.7914874409635,0.556024840834138));
#4287=CARTESIAN_POINT('Ctrl Pts',(-2.42404672820137,-26.3776775405011,0.613316507500758));
#4288=CARTESIAN_POINT('Ctrl Pts',(-2.05838114448734,-25.6376098899689,0.727899840834147));
#4289=CARTESIAN_POINT('Ctrl Pts',(-1.78223870534463,-25.3120853314176,0.785191507500833));
#4290=CARTESIAN_POINT('Ctrl Pts',(-1.10514273389326,-24.8279406528208,0.899774840834072));
#4291=CARTESIAN_POINT('Ctrl Pts',(-0.704807175805364,-24.6698281711569,
0.957066507500755));
#4292=CARTESIAN_POINT('Ctrl Pts',(0.1274352619041,-24.5613545958537,1.07164984083415));
#4293=CARTESIAN_POINT('Ctrl Pts',(0.558551263074086,-24.6111505358464,1.1289415075008));
#4294=CARTESIAN_POINT('Ctrl Pts',(1.35003809290966,-24.9104446162912,1.24352484083411));
#4295=CARTESIAN_POINT('Ctrl Pts',(1.70963130021051,-25.1597059023008,1.30081650750086));
#4296=CARTESIAN_POINT('Ctrl Pts',(2.27095531918287,-25.8021025401101,1.41539984083405));
#4297=CARTESIAN_POINT('Ctrl Pts',(2.4721077912595,-26.1946573298044,1.47269150750065));
#4298=CARTESIAN_POINT('Ctrl Pts',(2.66567502122425,-27.0325803320048,1.58727484083426));
#4299=CARTESIAN_POINT('Ctrl Pts',(2.65785211531719,-27.4771574273834,1.64456650750079));
#4300=CARTESIAN_POINT('Ctrl Pts',(2.43156425716401,-28.313995261359,1.75914984083412));
#4301=CARTESIAN_POINT('Ctrl Pts',(2.21326455198061,-28.7054399408851,1.81644150750076));
#4302=CARTESIAN_POINT('Ctrl Pts',(1.61433047837882,-29.3416770390113,1.93102484083414));
#4303=CARTESIAN_POINT('Ctrl Pts',(1.23423120401018,-29.5858229831059,1.98831650750076));
#4304=CARTESIAN_POINT('Ctrl Pts',(0.399489656769248,-29.8666031866432,2.10289984083414));
#4305=CARTESIAN_POINT('Ctrl Pts',(-0.0543696372039125,-29.902917630254,
2.16019150750069));
#4306=CARTESIAN_POINT('Ctrl Pts',(-0.929678265981594,-29.7557019006409,
2.27477484083421));
#4307=CARTESIAN_POINT('Ctrl Pts',(-1.3502798352523,-29.5722600576195,2.33206650750076));
#4308=CARTESIAN_POINT('Ctrl Pts',(-2.05817462844563,-29.0254285377532,2.44664984083415));
#4309=CARTESIAN_POINT('Ctrl Pts',(-2.344756721503,-28.6625205862691,2.50394150750071));
#4310=CARTESIAN_POINT('Ctrl Pts',(-2.71393246223352,-27.8401785078621,2.61852484083419));
#4311=CARTESIAN_POINT('Ctrl Pts',(-2.79612350398746,-27.3815105532419,2.67581650750078));
#4312=CARTESIAN_POINT('Ctrl Pts',(-2.73338114802542,-26.4753684673789,2.79039984083413));
#4313=CARTESIAN_POINT('Ctrl Pts',(-2.58845450226437,-26.0287664016884,2.84769150750084));
#4314=CARTESIAN_POINT('Ctrl Pts',(-2.10213141852588,-25.2534547274672,2.96227484083406));
#4315=CARTESIAN_POINT('Ctrl Pts',(-1.76115569452495,-24.9255165224303,3.01956650750075));
#4316=CARTESIAN_POINT('Ctrl Pts',(-0.960686964378836,-24.467748255277,3.13414984083416));
#4317=CARTESIAN_POINT('Ctrl Pts',(-0.501934458430937,-24.3384033014538,
3.19144150750079));
#4318=CARTESIAN_POINT('Ctrl Pts',(0.426712539268184,-24.3120260798245,3.30602484083412));
#4319=CARTESIAN_POINT('Ctrl Pts',(0.895718683084721,-24.4150725699735,3.36331650750083));
#4320=CARTESIAN_POINT('Ctrl Pts',(1.73323702163241,-24.8328266315758,3.47789984083408));
#4321=CARTESIAN_POINT('Ctrl Pts',(2.10092281068118,-25.1471817826938,3.53519150750045));
#4322=CARTESIAN_POINT('Ctrl Pts',(2.64645698476389,-25.9161536267569,3.64977484083445));
#4323=CARTESIAN_POINT('Ctrl Pts',(2.82373900440322,-26.3700644545806,3.707066507501));
#4324=CARTESIAN_POINT('Ctrl Pts',(2.94304329464034,-27.3122729858732,3.82164984083391));
#4325=CARTESIAN_POINT('Ctrl Pts',(2.8848981704904,-27.7996746143093,3.8789415075005));
#4326=CARTESIAN_POINT('Ctrl Pts',(2.54331827017279,-28.6932484441219,3.9935248408344));
#4327=CARTESIAN_POINT('Ctrl Pts',(2.26016080009324,-29.098545364816,4.05081650750084));
#4328=CARTESIAN_POINT('Ctrl Pts',(1.53234791989732,-29.7299686823744,4.16539984083407));
#4329=CARTESIAN_POINT('Ctrl Pts',(1.08835478333162,-29.9554496805941,4.2226915075008));
#4330=CARTESIAN_POINT('Ctrl Pts',(0.142056800052153,-30.1705740346633,4.33727484083411));
#4331=CARTESIAN_POINT('Ctrl Pts',(-0.359353255069153,-30.1599591044282,
4.39456650750057));
#4332=CARTESIAN_POINT('Ctrl Pts',(-1.30193124735312,-29.90159531999,4.50914984083433));
#4333=CARTESIAN_POINT('Ctrl Pts',(-1.74218197143407,-29.6540423974143,4.5664415075008));
#4334=CARTESIAN_POINT('Ctrl Pts',(-2.45655307667468,-28.9769743167667,4.6810248408341));
#4335=CARTESIAN_POINT('Ctrl Pts',(-2.72995223807354,-28.5480689977977,4.73831650750067));
#4336=CARTESIAN_POINT('Ctrl Pts',(-3.04280836800334,-27.6075872922707,4.85289984083423));
#4337=CARTESIAN_POINT('Ctrl Pts',(-3.08191483583748,-27.0968950385639,4.91019150750054));
#4338=CARTESIAN_POINT('Ctrl Pts',(-2.91314198222165,-26.1132114286668,5.02477484083437));
#4339=CARTESIAN_POINT('Ctrl Pts',(-2.70537161297122,-25.6411715125808,5.08206650750075));
#4340=CARTESIAN_POINT('Ctrl Pts',(-2.088440794589,-24.847860476929,5.19664984083415));
#4341=CARTESIAN_POINT('Ctrl Pts',(-1.67982912966058,-24.527382199886,5.25394150750074));
#4342=CARTESIAN_POINT('Ctrl Pts',(-0.755400051308564,-24.1159206391859,
5.36852484083416));
#4343=CARTESIAN_POINT('Ctrl Pts',(-0.240446469424114,-24.025380413375,5.42581650750074));
#4344=CARTESIAN_POINT('Ctrl Pts',(0.7756617100578,-24.0989534841673,5.54039984083416));
#4345=CARTESIAN_POINT('Ctrl Pts',(1.27583904542581,-24.2630496679924,5.59769150750081));
#4346=CARTESIAN_POINT('Ctrl Pts',(2.14302659233962,-24.8107622471434,5.71227484083409));
#4347=CARTESIAN_POINT('Ctrl Pts',(2.50917750925817,-25.1938992016932,5.76956650750086));
#4348=CARTESIAN_POINT('Ctrl Pts',(3.01903425440591,-26.0918186198254,5.88414984083404));
#4349=CARTESIAN_POINT('Ctrl Pts',(3.16220514490754,-26.6057673592151,5.94144150750084));
#4350=CARTESIAN_POINT('Ctrl Pts',(3.18858236658479,-27.644912529427,6.05602484083406));
#4351=CARTESIAN_POINT('Ctrl Pts',(3.07170993966424,-28.1691149066568,6.11331650750058));
#4352=CARTESIAN_POINT('Ctrl Pts',(2.60186740015778,-29.1040839332475,6.22789984083432));
#4353=CARTESIAN_POINT('Ctrl Pts',(2.2492995370817,-29.5139309527772,6.28519150750051));
#4354=CARTESIAN_POINT('Ctrl Pts',(1.38845182038838,-30.1208546223513,6.39977484083439));
#4355=CARTESIAN_POINT('Ctrl Pts',(0.880965722855629,-30.3173061799665,6.45706650750086));
#4356=CARTESIAN_POINT('Ctrl Pts',(-0.171208902055053,-30.4474411851313,
6.57164984083404));
#4357=CARTESIAN_POINT('Ctrl Pts',(-0.714896157737991,-30.3809468768386,
6.62894150750064));
#4358=CARTESIAN_POINT('Ctrl Pts',(-1.71055698753139,-29.9970811566254,6.74352484083427));
#4359=CARTESIAN_POINT('Ctrl Pts',(-2.16155762161384,-29.680027502494,6.80081650750078));
#4360=CARTESIAN_POINT('Ctrl Pts',(-2.86308023776419,-28.8667983798979,6.91539984083413));
#4361=CARTESIAN_POINT('Ctrl Pts',(-3.11288976212293,-28.3713668964897,6.97269150750051));
#4362=CARTESIAN_POINT('Ctrl Pts',(-3.34957124029864,-27.316693932087,7.0872748408344));
#4363=CARTESIAN_POINT('Ctrl Pts',(-3.33616428574757,-26.7584509172524,7.14456650750097));
#4364=CARTESIAN_POINT('Ctrl Pts',(-3.0457245749983,-25.7101327666455,7.25914984083393));
#4365=CARTESIAN_POINT('Ctrl Pts',(-2.76891843505522,-25.2210759980313,7.316441507501));
#4366=CARTESIAN_POINT('Ctrl Pts',(-2.01371634733806,-24.4285708856475,7.4310248408339));
#4367=CARTESIAN_POINT('Ctrl Pts',(-1.53600498378822,-24.1259185069575,7.48831650750057));
#4368=CARTESIAN_POINT('Ctrl Pts',(-0.48978311995981,-23.7809864506379,7.60289984083434));
#4369=CARTESIAN_POINT('Ctrl Pts',(0.0777420934653123,-23.7390879585698,
7.66019150750093));
#4370=CARTESIAN_POINT('Ctrl Pts',(1.16980068449715,-23.9294179362069,7.77477484083397));
#4371=CARTESIAN_POINT('Ctrl Pts',(1.69327894738216,-24.1615168316733,7.83206650750108));
#4372=CARTESIAN_POINT('Ctrl Pts',(2.57200622550959,-24.848546948579,7.94664984083383));
#4373=CARTESIAN_POINT('Ctrl Pts',(2.92638068652453,-25.3028623269368,8.00394150750066));
#4374=CARTESIAN_POINT('Ctrl Pts',(3.38012806720446,-26.3293784052561,8.11852484083425));
#4375=CARTESIAN_POINT('Ctrl Pts',(3.47901747707488,-26.9006176143865,8.17581650750176));
#4376=CARTESIAN_POINT('Ctrl Pts',(3.39461369143692,-28.0266918875018,8.29039984083314));
#4377=CARTESIAN_POINT('Ctrl Pts',(3.2113479695612,-28.5804444925376,8.347691507501));
#4378=CARTESIAN_POINT('Ctrl Pts',(2.60224589498633,-29.5395079121489,8.4622748408339));
#4379=CARTESIAN_POINT('Ctrl Pts',(2.17694770990781,-29.943871540951,8.51956650750176));
#4380=CARTESIAN_POINT('Ctrl Pts',(1.1815776037604,-30.5058167640846,8.63414984083314));
#4381=CARTESIAN_POINT('Ctrl Pts',(0.612432630957585,-30.6628135912745,8.69144150749966));
#4382=CARTESIAN_POINT('Ctrl Pts',(-0.537210711795104,-30.6891908129884,
8.80602484083524));
#4383=CARTESIAN_POINT('Ctrl Pts',(-1.11660932242181,-30.5584924493121,8.86331650750108));
#4384=CARTESIAN_POINT('Ctrl Pts',(-2.14902903706022,-30.0365614318812,8.97789984083382));
#4385=CARTESIAN_POINT('Ctrl Pts',(-2.60103728706707,-29.6457808568702,9.03519150750054));
#4386=CARTESIAN_POINT('Ctrl Pts',(-3.26935045213561,-28.6930572675207,9.14977484083436));
#4387=CARTESIAN_POINT('Ctrl Pts',(-3.48497154772812,-28.1319959002986,9.20706650750054));
#4388=CARTESIAN_POINT('Ctrl Pts',(-3.62593726781443,-26.9698551817563,9.32164984083436));
#4389=CARTESIAN_POINT('Ctrl Pts',(-3.55109377538202,-26.3698822988422,9.37894150750082));
#4390=CARTESIAN_POINT('Ctrl Pts',(-3.12494223527345,-25.2721344690503,9.49352484083408));
#4391=CARTESIAN_POINT('Ctrl Pts',(-2.77399239711041,-24.7754301215948,9.55081650750067));
#4392=CARTESIAN_POINT('Ctrl Pts',(-1.87534703207357,-24.0038082068396,9.66539984083423));
#4393=CARTESIAN_POINT('Ctrl Pts',(-1.328477201847,-23.7296701563417,9.72269150750066));
#4394=CARTESIAN_POINT('Ctrl Pts',(-0.165429256313216,-23.4714315540725,
9.83727484083425));
#4395=CARTESIAN_POINT('Ctrl Pts',(0.449646718215928,-23.487630532928,9.8945665075004));
#4396=CARTESIAN_POINT('Ctrl Pts',(1.60370502717545,-23.8101461699985,10.0091498408345));
#4397=CARTESIAN_POINT('Ctrl Pts',(2.14156784031432,-24.1162055272932,10.0664415075007));
#4398=CARTESIAN_POINT('Ctrl Pts',(3.01220695982868,-24.9495416221013,10.1810248408342));
#4399=CARTESIAN_POINT('Ctrl Pts',(3.344112555819,-25.4760590302157,10.2383165075002));
#4400=CARTESIAN_POINT('Ctrl Pts',(3.7211205385227,-26.6280210523566,10.3528998408347));
#4401=CARTESIAN_POINT('Ctrl Pts',(3.76581105482833,-27.2523792254888,10.4101915074991));
#4402=CARTESIAN_POINT('Ctrl Pts',(3.55392395316851,-28.4528127976668,10.5247748408358));
#4403=CARTESIAN_POINT('Ctrl Pts',(3.29749653150255,-29.0277294073495,10.5820665075001));
#4404=CARTESIAN_POINT('Ctrl Pts',(2.54036711604196,-29.9918729279439,10.6966498408348));
#4405=CARTESIAN_POINT('Ctrl Pts',(2.040348024276,-30.3801435729391,10.7539415075002));
#4406=CARTESIAN_POINT('Ctrl Pts',(0.911744945978275,-30.8761767735908,10.8685248408347));
#4407=CARTESIAN_POINT('Ctrl Pts',(0.284220109610612,-30.9834153675301,10.9258165075008));
#4408=CARTESIAN_POINT('Ctrl Pts',(-0.951820257144186,-30.8881808670358,
11.0403998408341));
#4409=CARTESIAN_POINT('Ctrl Pts',(-1.55914813184147,-30.6857456071259,11.0976915075009));
#4410=CARTESIAN_POINT('Ctrl Pts',(-2.61008742415662,-30.015254037105,11.212274840834));
#4411=CARTESIAN_POINT('Ctrl Pts',(-3.05266376483645,-29.5477946215084,11.2695665075011));
#4412=CARTESIAN_POINT('Ctrl Pts',(-3.6666974659612,-28.4549738273466,11.3841498408338));
#4413=CARTESIAN_POINT('Ctrl Pts',(-3.83752022944408,-27.8306326302477,11.4414415074993));
#4414=CARTESIAN_POINT('Ctrl Pts',(-3.85070884071214,-27.2005618634835,11.4987331741675));
#4415=CARTESIAN_POINT('Ctrl Pts',(-2.50007468503749,-27.1010187070962,-0.496297400879471));
#4416=CARTESIAN_POINT('Ctrl Pts',(-2.49697558534321,-26.6919449367377,-0.439005734212785));
#4417=CARTESIAN_POINT('Ctrl Pts',(-2.39148306502197,-26.2822116441738,-0.381714067546166));
#4418=CARTESIAN_POINT('Ctrl Pts',(-1.99708913925533,-25.5575010913513,-0.267130734212776));
#4419=CARTESIAN_POINT('Ctrl Pts',(-1.70851780633352,-25.2432423319883,-0.209839067546131));
#4420=CARTESIAN_POINT('Ctrl Pts',(-1.01332498488648,-24.7861838511185,-0.0952557342128104));
#4421=CARTESIAN_POINT('Ctrl Pts',(-0.607338782057628,-24.6438658572855,
-0.0379640675461273));
#4422=CARTESIAN_POINT('Ctrl Pts',(0.22809530726186,-24.5678109717687,0.0766192657871858));
#4423=CARTESIAN_POINT('Ctrl Pts',(0.656749262161081,-24.6342001019302,0.133910932453873));
#4424=CARTESIAN_POINT('Ctrl Pts',(1.43576881284334,-24.9635894484093,0.248494265787185));
#4425=CARTESIAN_POINT('Ctrl Pts',(1.78536871348538,-25.226324021095,0.305785932453894));
#4426=CARTESIAN_POINT('Ctrl Pts',(2.32151076365989,-25.8893852792693,0.420369265787164));
#4427=CARTESIAN_POINT('Ctrl Pts',(2.50749866272339,-26.2891116348328,0.477660932453768));
#4428=CARTESIAN_POINT('Ctrl Pts',(2.6691161443131,-27.1333885072357,0.592244265787291));
#4429=CARTESIAN_POINT('Ctrl Pts',(2.64453862625626,-27.577141828817,0.649535932453863));
#4430=CARTESIAN_POINT('Ctrl Pts',(2.38707841193931,-28.4045222689121,0.764119265787196));
#4431=CARTESIAN_POINT('Ctrl Pts',(2.15439078230601,-28.7873423753173,0.821410932453838));
#4432=CARTESIAN_POINT('Ctrl Pts',(1.53242332955732,-29.4005442496924,0.93599426578722));
#4433=CARTESIAN_POINT('Ctrl Pts',(1.14370063429288,-29.6303015787241,0.993285932453714));
#4434=CARTESIAN_POINT('Ctrl Pts',(0.299504189499764,-29.8799086688388,1.10786926578734));
#4435=CARTESIAN_POINT('Ctrl Pts',(-0.155177536543765,-29.8994684343923,
1.16516093245394));
#4436=CARTESIAN_POINT('Ctrl Pts',(-1.02412973658168,-29.7203034653188,1.27974426578712));
#4437=CARTESIAN_POINT('Ctrl Pts',(-1.43755852562162,-29.5216976236493,1.33703593245383));
#4438=CARTESIAN_POINT('Ctrl Pts',(-2.1247866819161,-28.9496857898884,1.45161926578722));
#4439=CARTESIAN_POINT('Ctrl Pts',(-2.39789468808455,-28.576785610739,1.50891093245379));
#4440=CARTESIAN_POINT('Ctrl Pts',(-2.73697416446945,-27.7419786632607,1.62349426578727));
#4441=CARTESIAN_POINT('Ctrl Pts',(-2.80257181896535,-27.280849991177,1.68078593245385));
#4442=CARTESIAN_POINT('Ctrl Pts',(-2.70741102889003,-26.3779021530229,1.7953692657872));
#4443=CARTESIAN_POINT('Ctrl Pts',(-2.54669034787763,-25.9369519968831,1.85266093245392));
#4444=CARTESIAN_POINT('Ctrl Pts',(-2.03328251568525,-25.1797393416946,1.96724426578714));
#4445=CARTESIAN_POINT('Ctrl Pts',(-1.6810419878648,-24.8642309325484,2.02453593245391));
#4446=CARTESIAN_POINT('Ctrl Pts',(-0.86521846062969,-24.4351922371926,2.13911926578715));
#4447=CARTESIAN_POINT('Ctrl Pts',(-0.402390649877755,-24.322119576435,2.19641093245378));
#4448=CARTESIAN_POINT('Ctrl Pts',(0.526255043490125,-24.3283177763288,2.31099426578728));
#4449=CARTESIAN_POINT('Ctrl Pts',(0.991184579421847,-24.4476362331387,2.36828593245382));
#4450=CARTESIAN_POINT('Ctrl Pts',(1.81334582024015,-24.8941186368221,2.48286926578724));
#4451=CARTESIAN_POINT('Ctrl Pts',(2.16976581012525,-25.2209026816946,2.54016093245371));
#4452=CARTESIAN_POINT('Ctrl Pts',(2.68821378645142,-26.007971375774,2.65474426578735));
#4453=CARTESIAN_POINT('Ctrl Pts',(2.84970131829056,-26.4675328483271,2.71203593245399));
#4454=CARTESIAN_POINT('Ctrl Pts',(2.93658691870944,-27.4129330312322,2.82661926578707));
#4455=CARTESIAN_POINT('Ctrl Pts',(2.86184860442354,-27.897872613403,2.88391093245367));
#4456=CARTESIAN_POINT('Ctrl Pts',(2.49017343803774,-28.7789791640489,2.99849426578739));
#4457=CARTESIAN_POINT('Ctrl Pts',(2.19354268131092,-29.1742827781052,3.05578593245391));
#4458=CARTESIAN_POINT('Ctrl Pts',(1.44506518072621,-29.7805241268371,3.17036926578715));
#4459=CARTESIAN_POINT('Ctrl Pts',(0.993900478307379,-29.9908405520754,3.22766093245387));
#4460=CARTESIAN_POINT('Ctrl Pts',(0.0412486248171475,-30.1740151577347,
3.34224426578718));
#4461=CARTESIAN_POINT('Ctrl Pts',(-0.459337656509201,-30.1466456153845,
3.39953593245365));
#4462=CARTESIAN_POINT('Ctrl Pts',(-1.39245825489971,-29.8571094747481,3.51411926578741));
#4463=CARTESIAN_POINT('Ctrl Pts',(-1.82408440587509,-29.5951686277527,3.57141093245388));
#4464=CARTESIAN_POINT('Ctrl Pts',(-2.51542028734699,-28.8950671679322,3.68599426578718));
#4465=CARTESIAN_POINT('Ctrl Pts',(-2.77443083370738,-28.4575384280859,3.74328593245375));
#4466=CARTESIAN_POINT('Ctrl Pts',(-3.05611385018328,-27.5076018249958,3.85786926578731));
#4467=CARTESIAN_POINT('Ctrl Pts',(-3.07846563998978,-26.9960871392191,3.91516093245361));
#4468=CARTESIAN_POINT('Ctrl Pts',(-2.87774354688549,-26.0187599580717,4.02974426578744));
#4469=CARTESIAN_POINT('Ctrl Pts',(-2.65480917901121,-25.5538928222013,4.08703593245365));
#4470=CARTESIAN_POINT('Ctrl Pts',(-2.01269804671401,-24.7812484234687,4.20161926578741));
#4471=CARTESIAN_POINT('Ctrl Pts',(-1.59409415413557,-24.4742442332878,4.25891093245382));
#4472=CARTESIAN_POINT('Ctrl Pts',(-0.657200206702104,-24.0928789369666,
4.37349426578724));
#4473=CARTESIAN_POINT('Ctrl Pts',(-0.139785907354555,-24.0189320983815,
4.43078593245364));
#4474=CARTESIAN_POINT('Ctrl Pts',(0.873128024409321,-24.1249236033184,4.54536926578742));
#4475=CARTESIAN_POINT('Ctrl Pts',(1.36765345024244,-24.3048138223663,4.60266093245389));
#4476=CARTESIAN_POINT('Ctrl Pts',(2.21674197810085,-24.8796111499969,4.71724426578717));
#4477=CARTESIAN_POINT('Ctrl Pts',(2.57046309915192,-25.2740129083479,4.77453593245413));
#4478=CARTESIAN_POINT('Ctrl Pts',(3.05159027247857,-26.1872871235801,4.88911926578693));
#4479=CARTESIAN_POINT('Ctrl Pts',(3.1784888699414,-26.7053111677683,4.94641093245373));
#4480=CARTESIAN_POINT('Ctrl Pts',(3.17229067006551,-27.7444550336489,5.06099426578732));
#4481=CARTESIAN_POINT('Ctrl Pts',(3.03914627651117,-28.2645808029984,5.11828593245366));
#4482=CARTESIAN_POINT('Ctrl Pts',(2.54057539489944,-29.1841927318507,5.2328692657874));
#4483=CARTESIAN_POINT('Ctrl Pts',(2.17557863808745,-29.5827739522296,5.29016093245358));
#4484=CARTESIAN_POINT('Ctrl Pts',(1.29663407136474,-30.1626114240305,5.40474426578747));
#4485=CARTESIAN_POINT('Ctrl Pts',(0.783497329111631,-30.3432684938695,5.46203593245413));
#4486=CARTESIAN_POINT('Ctrl Pts',(-0.271868947416543,-30.4409848091847,
5.57661926578693));
#4487=CARTESIAN_POINT('Ctrl Pts',(-0.813094156837556,-30.3578973107856,
5.63391093245353));
#4488=CARTESIAN_POINT('Ctrl Pts',(-1.7962877074525,-29.9439363244765,5.74849426578753));
#4489=CARTESIAN_POINT('Ctrl Pts',(-2.23729503491243,-29.613409383722,5.80578593245404));
#4490=CARTESIAN_POINT('Ctrl Pts',(-2.91363568221747,-28.7795156407165,5.92036926578702));
#4491=CARTESIAN_POINT('Ctrl Pts',(-3.14828063361543,-28.2769125914658,5.97766093245358));
#4492=CARTESIAN_POINT('Ctrl Pts',(-3.35301236335888,-27.2158857568516,6.09224426578747));
#4493=CARTESIAN_POINT('Ctrl Pts',(-3.32285079671477,-26.6584665158089,6.14953593245386));
#4494=CARTESIAN_POINT('Ctrl Pts',(-3.00123872974546,-25.6196057591023,6.2641192657872));
#4495=CARTESIAN_POINT('Ctrl Pts',(-2.71004466540204,-25.1391735635767,6.32141093245427));
#4496=CARTESIAN_POINT('Ctrl Pts',(-1.93180919849512,-24.3697036749888,6.43599426578679));
#4497=CARTESIAN_POINT('Ctrl Pts',(-1.44547441408027,-24.0814399113125,6.49328593245345));
#4498=CARTESIAN_POINT('Ctrl Pts',(-0.389797652680968,-23.7676809684691,
6.60786926578761));
#4499=CARTESIAN_POINT('Ctrl Pts',(0.178549992812208,-23.7425371544047,6.66516093245401));
#4500=CARTESIAN_POINT('Ctrl Pts',(1.26425215509018,-23.9648163715558,6.77974426578705));
#4501=CARTESIAN_POINT('Ctrl Pts',(1.7805576377681,-24.2120792656227,6.83703593245416));
#4502=CARTESIAN_POINT('Ctrl Pts',(2.63861827896344,-24.9242896964646,6.9516192657869));
#4503=CARTESIAN_POINT('Ctrl Pts',(2.9795186531323,-25.3885973024572,7.00891093245373));
#4504=CARTESIAN_POINT('Ctrl Pts',(3.40316976941416,-26.4275782498672,7.12349426578732));
#4505=CARTESIAN_POINT('Ctrl Pts',(3.4854657920787,-27.0012781764557,7.18078593245407));
#4506=CARTESIAN_POINT('Ctrl Pts',(3.36864357227559,-28.1241582018537,7.29536926578699));
#4507=CARTESIAN_POINT('Ctrl Pts',(3.16958381519666,-28.6722588973589,7.35266093245407));
#4508=CARTESIAN_POINT('Ctrl Pts',(2.53339699212349,-29.6132232979053,7.46724426578698));
#4509=CARTESIAN_POINT('Ctrl Pts',(2.09683400325949,-30.0051571308579,7.52453593245425));
#4510=CARTESIAN_POINT('Ctrl Pts',(1.08610909999943,-30.538372782144,7.63911926578681));
#4511=CARTESIAN_POINT('Ctrl Pts',(0.512888822404401,-30.6790973163175,7.69641093245254));
#4512=CARTESIAN_POINT('Ctrl Pts',(-0.636753216017042,-30.67289911646,7.81099426578851));
#4513=CARTESIAN_POINT('Ctrl Pts',(-1.21207521877181,-30.5259287861701,7.86828593245416));
#4514=CARTESIAN_POINT('Ctrl Pts',(-2.22913783565509,-29.9752694266119,7.9828692657869));
#4515=CARTESIAN_POINT('Ctrl Pts',(-2.66988028653065,-29.5720599578842,8.04016093245362));
#4516=CARTESIAN_POINT('Ctrl Pts',(-3.31110725380362,-28.6012395184888,8.15474426578744));
#4517=CARTESIAN_POINT('Ctrl Pts',(-3.51093386164047,-28.034527506556,8.21203593245362));
#4518=CARTESIAN_POINT('Ctrl Pts',(-3.61948089185851,-26.8691951363934,8.32661926578744));
#4519=CARTESIAN_POINT('Ctrl Pts',(-3.52804420933835,-26.2716842997393,8.3839109324539));
#4520=CARTESIAN_POINT('Ctrl Pts',(-3.07179740311519,-25.1864037491325,8.49849426578716));
#4521=CARTESIAN_POINT('Ctrl Pts',(-2.70737427834283,-24.6996927082866,8.55578593245375));
#4522=CARTESIAN_POINT('Ctrl Pts',(-1.78806429288772,-23.9532527623958,8.67036926578731));
#4523=CARTESIAN_POINT('Ctrl Pts',(-1.2340228968259,-23.6942792848374,8.72766093245373));
#4524=CARTESIAN_POINT('Ctrl Pts',(-0.0646210810750642,-23.467990431024,
8.84224426578733));
#4525=CARTESIAN_POINT('Ctrl Pts',(0.549631119664167,-23.5009440219499,8.89953593245347));
#4526=CARTESIAN_POINT('Ctrl Pts',(1.69423203471385,-23.8546320152623,9.01411926578758));
#4527=CARTESIAN_POINT('Ctrl Pts',(2.22347027477345,-24.1750792969402,9.07141093245382));
#4528=CARTESIAN_POINT('Ctrl Pts',(3.07107417048285,-25.0314487709504,9.18599426578724));
#4529=CARTESIAN_POINT('Ctrl Pts',(3.38859115147477,-25.5665895999213,9.2432859324533));
#4530=CARTESIAN_POINT('Ctrl Pts',(3.73442602068069,-26.7280065196379,9.35786926578775));
#4531=CARTESIAN_POINT('Ctrl Pts',(3.76236185900407,-27.3531871248382,9.41516093245296));
#4532=CARTESIAN_POINT('Ctrl Pts',(3.5185255178089,-28.5472642682574,9.5297442657881));
#4533=CARTESIAN_POINT('Ctrl Pts',(3.24693409756131,-29.1150080977418,9.58703593245323));
#4534=CARTESIAN_POINT('Ctrl Pts',(2.46462436814819,-30.0584849813914,9.70161926578783));
#4535=CARTESIAN_POINT('Ctrl Pts',(1.95461304876198,-30.4332815395597,9.75891093245325));
#4536=CARTESIAN_POINT('Ctrl Pts',(0.813545101360808,-30.8992184757877,9.8734942657878));
#4537=CARTESIAN_POINT('Ctrl Pts',(0.183559547541048,-30.9898636825423,9.93078593245385));
#4538=CARTESIAN_POINT('Ctrl Pts',(-1.0492865714957,-30.8622107478662,10.0453692657872));
#4539=CARTESIAN_POINT('Ctrl Pts',(-1.65096253667027,-30.6439814527683,10.102660932454));
#4540=CARTESIAN_POINT('Ctrl Pts',(-2.68380280990567,-29.9464051342351,10.2172442657871));
#4541=CARTESIAN_POINT('Ctrl Pts',(-3.11394935474709,-29.4676809148667,10.2745359324542));
#4542=CARTESIAN_POINT('Ctrl Pts',(-3.69925348401698,-28.3595053235791,10.3891192657869));
#4543=CARTESIAN_POINT('Ctrl Pts',(-3.85380395473586,-27.7310888216945,10.4464109324524));
#4544=CARTESIAN_POINT('Ctrl Pts',(-3.85070485496943,-27.1010187070959,10.5037025991205));
#4545=CARTESIAN_POINT('Ctrl Pts',(-3.49999867141204,-27.1131792015256,-0.497516610416937));
#4546=CARTESIAN_POINT('Ctrl Pts',(-3.49888932799759,-26.5404932488512,-0.440224943750252));
#4547=CARTESIAN_POINT('Ctrl Pts',(-3.35444114738347,-25.9668063623456,-0.382933277083632));
#4548=CARTESIAN_POINT('Ctrl Pts',(-2.80930434430968,-24.9516337619221,-0.268349943750243));
#4549=CARTESIAN_POINT('Ctrl Pts',(-2.40908999522195,-24.5111444093371,-0.211058277083598));
#4550=CARTESIAN_POINT('Ctrl Pts',(-1.44403096339936,-23.8689809726516,-0.0964749437502769));
#4551=CARTESIAN_POINT('Ctrl Pts',(-0.880079720887058,-23.6679656879623,
-0.0391832770835939));
#4552=CARTESIAN_POINT('Ctrl Pts',(0.28061299005863,-23.5558768567235,0.0754000562497192));
#4553=CARTESIAN_POINT('Ctrl Pts',(0.876249383825206,-23.6449638021555,0.132691722916406));
#4554=CARTESIAN_POINT('Ctrl Pts',(1.95910771378206,-24.0958998985319,0.247275056249719));
#4555=CARTESIAN_POINT('Ctrl Pts',(2.44527330196474,-24.4573671339349,0.304566722916428));
#4556=CARTESIAN_POINT('Ctrl Pts',(3.19208049125558,-25.370851664545,0.419150056249697));
#4557=CARTESIAN_POINT('Ctrl Pts',(3.4519663191088,-25.9220290742938,0.476441722916301));
#4558=CARTESIAN_POINT('Ctrl Pts',(3.68132515309603,-27.08646641491,0.591025056249824));
#4559=CARTESIAN_POINT('Ctrl Pts',(3.65052625709869,-27.6986228841538,0.648316722916396));
#4560=CARTESIAN_POINT('Ctrl Pts',(3.30188598195419,-28.8402927016588,0.762900056249729));
#4561=CARTESIAN_POINT('Ctrl Pts',(2.98432689255302,-29.3686983876925,0.820191722916372));
#4562=CARTESIAN_POINT('Ctrl Pts',(2.13379081833063,-30.216096764043,0.934775056249753));
#4563=CARTESIAN_POINT('Ctrl Pts',(1.60158961081322,-30.5342409823362,0.992066722916289));
#4564=CARTESIAN_POINT('Ctrl Pts',(0.445414171550833,-30.8826444452813,1.10665005624984));
#4565=CARTESIAN_POINT('Ctrl Pts',(-0.177469596581333,-30.912519185481,1.16394172291647));
#4566=CARTESIAN_POINT('Ctrl Pts',(-1.36813499365341,-30.6734189584949,1.27852505624965));
#4567=CARTESIAN_POINT('Ctrl Pts',(-1.93476718568864,-30.4046202185468,1.33581672291637));
#4568=CARTESIAN_POINT('Ctrl Pts',(-2.87746776648538,-29.6280956550586,1.45040005624976));
#4569=CARTESIAN_POINT('Ctrl Pts',(-3.25260040831661,-29.1210712820873,1.50769172291632));
#4570=CARTESIAN_POINT('Ctrl Pts',(-3.72057981489945,-27.9854713421496,1.6222750562498));
#4571=CARTESIAN_POINT('Ctrl Pts',(-3.81292945777313,-27.3579616111638,1.67956672291639));
#4572=CARTESIAN_POINT('Ctrl Pts',(-3.68965542200644,-26.1289750303032,1.79415005624974));
#4573=CARTESIAN_POINT('Ctrl Pts',(-3.47409640017873,-25.5286790803258,1.85144172291645));
#4574=CARTESIAN_POINT('Ctrl Pts',(-2.78220129939746,-24.4971784172052,1.96602505624967));
#4575=CARTESIAN_POINT('Ctrl Pts',(-2.30648258548237,-24.0669901790178,2.02331672291636));
#4576=CARTESIAN_POINT('Ctrl Pts',(-1.20394886875872,-23.4801893728762,2.13790005624977));
#4577=CARTESIAN_POINT('Ctrl Pts',(-0.578163322834367,-23.3241853462944,
2.1951917229164));
#4578=CARTESIAN_POINT('Ctrl Pts',(0.677706727587892,-23.3264040337203,2.30977505624973));
#4579=CARTESIAN_POINT('Ctrl Pts',(1.30658986109621,-23.4846781506972,2.36706672291644));
#4580=CARTESIAN_POINT('Ctrl Pts',(2.4192131498232,-24.0819034318477,2.48165005624969));
#4581=CARTESIAN_POINT('Ctrl Pts',(2.9018637326796,-24.5203304926646,2.53894172291615));
#4582=CARTESIAN_POINT('Ctrl Pts',(3.60541666501523,-25.5772653974027,2.65352505624997));
#4583=CARTESIAN_POINT('Ctrl Pts',(3.82560148759511,-26.1947919093305,2.71081672291652));
#4584=CARTESIAN_POINT('Ctrl Pts',(3.94852103377322,-27.4654507141961,2.8254000562496));
#4585=CARTESIAN_POINT('Ctrl Pts',(3.85108490425945,-28.1173727349135,2.88269172291611));
#4586=CARTESIAN_POINT('Ctrl Pts',(3.35786298785392,-29.3023180651413,2.99727505625001));
#4587=CARTESIAN_POINT('Ctrl Pts',(2.96249956859728,-29.8341873664785,3.05456672291645));
#4588=CARTESIAN_POINT('Ctrl Pts',(1.96359879532417,-30.6510938545388,3.16915005624968));
#4589=CARTESIAN_POINT('Ctrl Pts',(1.36098303900346,-30.9353082084263,3.22644172291641));
#4590=CARTESIAN_POINT('Ctrl Pts',(0.0881707169855854,-31.1862241665521,
3.34102505624972));
#4591=CARTESIAN_POINT('Ctrl Pts',(-0.580818711692515,-31.1526332462716,
3.39831672291618));
#4592=CARTESIAN_POINT('Ctrl Pts',(-1.82822868779995,-30.7719170447183,3.51290005624994));
#4593=CARTESIAN_POINT('Ctrl Pts',(-2.40544041813704,-30.4251047381095,3.57019172291641));
#4594=CARTESIAN_POINT('Ctrl Pts',(-3.33097280181086,-29.4964346565957,3.68477505624972));
#4595=CARTESIAN_POINT('Ctrl Pts',(-3.67837023727213,-28.9154274047545,3.74206672291629));
#4596=CARTESIAN_POINT('Ctrl Pts',(-4.05884962667304,-27.6535118068985,3.85665005624984));
#4597=CARTESIAN_POINT('Ctrl Pts',(-4.09151639110769,-26.9737950793345,3.91394172291615));
#4598=CARTESIAN_POINT('Ctrl Pts',(-3.83085904003235,-25.6747547008469,4.02852505624998));
#4599=CARTESIAN_POINT('Ctrl Pts',(-3.53773177400349,-25.0566841622527,4.08581672291636));
#4600=CARTESIAN_POINT('Ctrl Pts',(-2.69110791178932,-24.028567338781,4.20040005624976));
#4601=CARTESIAN_POINT('Ctrl Pts',(-2.13837982562106,-23.6195385131152,4.25769172291635));
#4602=CARTESIAN_POINT('Ctrl Pts',(-0.900692885453703,-23.1092732864771,
4.37227505624977));
#4603=CARTESIAN_POINT('Ctrl Pts',(-0.216897527488987,-23.0085744595606,
4.42956672291635));
#4604=CARTESIAN_POINT('Ctrl Pts',(1.12205514727662,-23.142679210215,4.54415005624977));
#4605=CARTESIAN_POINT('Ctrl Pts',(1.775926366677,-23.3774077699852,4.60144172291642));
#4606=CARTESIAN_POINT('Ctrl Pts',(2.89930290271304,-24.1306923663646,4.71602505624971));
#4607=CARTESIAN_POINT('Ctrl Pts',(3.36770385261388,-24.6485723106026,4.77331672291647));
#4608=CARTESIAN_POINT('Ctrl Pts',(4.00659313686357,-25.8485567155787,4.88790005624965));
#4609=CARTESIAN_POINT('Ctrl Pts',(4.17642310008015,-26.5295384946699,4.94519172291645));
#4610=CARTESIAN_POINT('Ctrl Pts',(4.17420441267586,-27.8959067178885,5.05977505624967));
#4611=CARTESIAN_POINT('Ctrl Pts',(4.00210435901772,-28.5799860845476,5.11706672291619));
#4612=CARTESIAN_POINT('Ctrl Pts',(3.3527905998087,-29.7900600615589,5.23165005624993));
#4613=CARTESIAN_POINT('Ctrl Pts',(2.87615082723203,-30.314871874706,5.28894172291612));
#4614=CARTESIAN_POINT('Ctrl Pts',(1.72734004962141,-31.0798143026723,5.40352505625001));
#4615=CARTESIAN_POINT('Ctrl Pts',(1.05623826824525,-31.3191686631573,5.46081672291647));
#4616=CARTESIAN_POINT('Ctrl Pts',(-0.324386630517576,-31.4529189242652,
5.57540005624965));
#4617=CARTESIAN_POINT('Ctrl Pts',(-1.03259427822014,-31.3471336106709,5.63269172291625));
#4618=CARTESIAN_POINT('Ctrl Pts',(-2.31962660867283,-30.8116258742433,5.74727505624988));
#4619=CARTESIAN_POINT('Ctrl Pts',(-2.89719962320057,-30.3823662711092,5.80456672291639));
#4620=CARTESIAN_POINT('Ctrl Pts',(-3.78420541000443,-29.2980492552136,5.91915005624974));
#4621=CARTESIAN_POINT('Ctrl Pts',(-4.09274828993971,-28.6439951522933,5.97644172291612));
#4622=CARTESIAN_POINT('Ctrl Pts',(-4.36522137220295,-27.2628078488887,6.09102505625001));
#4623=CARTESIAN_POINT('Ctrl Pts',(-4.32883842763837,-26.5369854607524,6.14831672291658));
#4624=CARTESIAN_POINT('Ctrl Pts',(-3.91604629967915,-25.1838353260752,6.26290005624954));
#4625=CARTESIAN_POINT('Ctrl Pts',(-3.53998077585005,-24.5578175514078,6.32019172291661));
#4626=CARTESIAN_POINT('Ctrl Pts',(-2.53317668706739,-23.5541511604319,6.43477505624951));
#4627=CARTESIAN_POINT('Ctrl Pts',(-1.90336339087076,-23.1775005077857,6.49206672291618));
#4628=CARTESIAN_POINT('Ctrl Pts',(-0.535707634461822,-22.7649451919414,
6.60665005624995));
#4629=CARTESIAN_POINT('Ctrl Pts',(0.200842052573385,-22.7294864032627,6.66394172291654));
#4630=CARTESIAN_POINT('Ctrl Pts',(1.60825741243838,-23.0117008784331,6.77852505624958));
#4631=CARTESIAN_POINT('Ctrl Pts',(2.27776629761871,-23.3291566705507,6.83581672291669));
#4632=CARTESIAN_POINT('Ctrl Pts',(3.39129936374918,-24.2458798314691,6.95040005624944));
#4633=CARTESIAN_POINT('Ctrl Pts',(3.8342243732566,-24.8443116308563,7.00769172291627));
#4634=CARTESIAN_POINT('Ctrl Pts',(4.38677541995195,-26.1840855712311,7.12227505624986));
#4635=CARTESIAN_POINT('Ctrl Pts',(4.49582343090945,-26.9241665562002,7.1795667229166));
#4636=CARTESIAN_POINT('Ctrl Pts',(4.35088796536903,-28.3730853248421,7.29415005624953));
#4637=CARTESIAN_POINT('Ctrl Pts',(4.09698986764256,-29.0805318136941,7.35144172291661));
#4638=CARTESIAN_POINT('Ctrl Pts',(3.28231577569086,-30.295784222617,7.46602505624951));
#4639=CARTESIAN_POINT('Ctrl Pts',(2.72227460111075,-30.8023978842609,7.52331672291659));
#4640=CARTESIAN_POINT('Ctrl Pts',(1.42483950789472,-31.4933756465881,7.63790005624954));
#4641=CARTESIAN_POINT('Ctrl Pts',(0.688661495622512,-31.6770315464534,7.69519172291528));
#4642=CARTESIAN_POINT('Ctrl Pts',(-0.788204900376376,-31.6748128590733,
7.80977505625085));
#4643=CARTESIAN_POINT('Ctrl Pts',(-1.52748050021878,-31.4888868687303,7.86706672291669));
#4644=CARTESIAN_POINT('Ctrl Pts',(-2.83500516546561,-30.7874846314674,7.98165005624943));
#4645=CARTESIAN_POINT('Ctrl Pts',(-3.40197820894101,-30.2726321471241,8.03894172291615));
#4646=CARTESIAN_POINT('Ctrl Pts',(-4.22831013251146,-29.0319454966501,8.15352505624997));
#4647=CARTESIAN_POINT('Ctrl Pts',(-4.48683403091752,-28.3072684458016,8.21081672291615));
#4648=CARTESIAN_POINT('Ctrl Pts',(-4.63141500694981,-26.8166774531803,8.32540005624997));
#4649=CARTESIAN_POINT('Ctrl Pts',(-4.51728050926608,-26.0521841784596,8.38269172291643));
#4650=CARTESIAN_POINT('Ctrl Pts',(-3.93948695283954,-24.6630648478093,8.49727505624969));
#4651=CARTESIAN_POINT('Ctrl Pts',(-3.47633116581651,-24.0397881200713,8.55456672291628));
#4652=CARTESIAN_POINT('Ctrl Pts',(-2.3065979072983,-23.082683034536,8.66915005624984));
#4653=CARTESIAN_POINT('Ctrl Pts',(-1.60110545776092,-22.7498116285361,8.72644172291626));
#4654=CARTESIAN_POINT('Ctrl Pts',(-0.1115431730045,-22.455781422157,8.84102505624986));
#4655=CARTESIAN_POINT('Ctrl Pts',(0.671112174616573,-22.4949563909962,8.89831672291601));
#4656=CARTESIAN_POINT('Ctrl Pts',(2.13000246784507,-22.9398244453587,9.01290005625012));
#4657=CARTESIAN_POINT('Ctrl Pts',(2.80482628686612,-23.3451431864166,9.07019172291636));
#4658=CARTESIAN_POINT('Ctrl Pts',(3.88662668511606,-24.4300812824538,9.18477505624977));
#4659=CARTESIAN_POINT('Ctrl Pts',(4.29253055496877,-25.1087006230277,9.24206672291584));
#4660=CARTESIAN_POINT('Ctrl Pts',(4.73716179724122,-26.5820965379602,9.35665005625028));
#4661=CARTESIAN_POINT('Ctrl Pts',(4.77541261016421,-27.3754791844964,9.41394172291549));
#4662=CARTESIAN_POINT('Ctrl Pts',(4.47164101091353,-28.8912695257086,9.52852505625063));
#4663=CARTESIAN_POINT('Ctrl Pts',(4.12985669269715,-29.6122167575113,9.58581672291576));
#4664=CARTESIAN_POINT('Ctrl Pts',(3.1430342330799,-30.8111660662582,9.70040005625036));
#4665=CARTESIAN_POINT('Ctrl Pts',(2.49889872045615,-31.2879872596437,9.75769172291579));
#4666=CARTESIAN_POINT('Ctrl Pts',(1.05703777990366,-31.8828241263658,9.87227505625033));
#4667=CARTESIAN_POINT('Ctrl Pts',(0.260671167899412,-32.0002213213825,9.92956672291638));
#4668=CARTESIAN_POINT('Ctrl Pts',(-1.29821369458701,-31.8444551409501,10.0441500562497));
#4669=CARTESIAN_POINT('Ctrl Pts',(-2.05923545291888,-31.5713875052691,10.1014417229165));
#4670=CARTESIAN_POINT('Ctrl Pts',(-3.36636373470387,-30.6953239177476,10.2160250562496));
#4671=CARTESIAN_POINT('Ctrl Pts',(-3.91119010810414,-30.0931215128015,10.2733167229167));
#4672=CARTESIAN_POINT('Ctrl Pts',(-4.65425634850692,-28.6982357313908,10.3879000562494));
#4673=CARTESIAN_POINT('Ctrl Pts',(-4.85173818484261,-27.906861497377,10.4451917229149));
#4674=CARTESIAN_POINT('Ctrl Pts',(-4.85062884134398,-27.1131792015253,10.5024833895831));
#4675=CARTESIAN_POINT('Origin',(-3.5,-27.1629509039024,-4.33680868994202E-16));
#4676=CARTESIAN_POINT('Origin',(-4.85063016993195,-27.162950903902,11.));
#4677=CARTESIAN_POINT('Origin',(-3.5,-27.1629509039024,-4.33680868994202E-16));
#4678=CARTESIAN_POINT('Ctrl Pts',(-3.49996080530815,-27.2127230666419,22.4975165628198));
#4679=CARTESIAN_POINT('Ctrl Pts',(-3.49923858446785,-27.7853227106402,22.4402329418509));
#4680=CARTESIAN_POINT('Ctrl Pts',(-3.35442400014962,-28.3588108293565,22.3829524076267));
#4681=CARTESIAN_POINT('Ctrl Pts',(-2.53805890913148,-29.8820941336696,22.2111092614391));
#4682=CARTESIAN_POINT('Ctrl Pts',(-1.46143501137141,-30.6017071597437,22.0965431123954));
#4683=CARTESIAN_POINT('Ctrl Pts',(0.859993909463204,-30.8281716102345,21.8674140533199));
#4684=CARTESIAN_POINT('Ctrl Pts',(2.07105132984979,-30.3269875071567,21.7528496294383));
#4685=CARTESIAN_POINT('Ctrl Pts',(3.56717700801455,-28.5011027334814,21.5237158877512));
#4686=CARTESIAN_POINT('Ctrl Pts',(3.82655802944863,-27.2003585446699,21.4091531369767));
#4687=CARTESIAN_POINT('Ctrl Pts',(3.13176866916735,-24.9149704304093,21.1800148858282));
#4688=CARTESIAN_POINT('Ctrl Pts',(2.18340277243941,-23.9654078612039,21.0654537578317));
#4689=CARTESIAN_POINT('Ctrl Pts',(-0.129624475723444,-23.26492626726,20.8363111624828));
#4690=CARTESIAN_POINT('Ctrl Pts',(-1.46146161962901,-23.5287714044906,20.7217516085899));
#4691=CARTESIAN_POINT('Ctrl Pts',(-3.35087032746474,-25.0803824700087,20.4926048268444));
#4692=CARTESIAN_POINT('Ctrl Pts',(-3.87760724316326,-26.3487572317876,20.3780467999886));
#4693=CARTESIAN_POINT('Ctrl Pts',(-3.63476056023195,-28.8097599072106,20.1488959825923));
#4694=CARTESIAN_POINT('Ctrl Pts',(-2.86424004281594,-29.965541294796,20.0343394372402));
#4695=CARTESIAN_POINT('Ctrl Pts',(-0.658453525508203,-31.1444028451946,
19.8051847283177));
#4696=CARTESIAN_POINT('Ctrl Pts',(0.746295607863299,-31.1460497722331,19.6906296204221));
#4697=CARTESIAN_POINT('Ctrl Pts',(2.97686521751534,-29.9539838567283,19.4614711577696));
#4698=CARTESIAN_POINT('Ctrl Pts',(3.76753534062837,-28.7739677375461,19.3469174447372));
#4699=CARTESIAN_POINT('Ctrl Pts',(4.01866309430747,-26.2291292657398,19.1177553601879));
#4700=CARTESIAN_POINT('Ctrl Pts',(3.47096346939119,-24.9015823386939,19.0032030007967));
#4701=CARTESIAN_POINT('Ctrl Pts',(1.47301680764982,-23.2609008561182,18.7740374205694));
#4702=CARTESIAN_POINT('Ctrl Pts',(0.0495864900580295,-22.9755165719832,
18.6594863749187));
#4703=CARTESIAN_POINT('Ctrl Pts',(-2.45153366210842,-23.7331018039879,18.4303174198824));
#4704=CARTESIAN_POINT('Ctrl Pts',(-3.49083915992615,-24.7690401632385,18.3157676493834));
#4705=CARTESIAN_POINT('Ctrl Pts',(-4.25889868811986,-27.2963083875918,18.0865954352922));
#4706=CARTESIAN_POINT('Ctrl Pts',(-3.97206991737307,-28.7513902818761,17.9720469025882));
#4707=CARTESIAN_POINT('Ctrl Pts',(-2.27985145267618,-30.8159510369377,17.7428715404485));
#4708=CARTESIAN_POINT('Ctrl Pts',(-0.896239671425334,-31.3920117915409,
17.6283242093665));
#4709=CARTESIAN_POINT('Ctrl Pts',(1.11729400206607,-31.1951401445063,17.4564404065291));
#4710=CARTESIAN_POINT('Ctrl Pts',(1.77292736544793,-30.9607175289896,17.3991671837723));
#4711=CARTESIAN_POINT('Ctrl Pts',(2.90077819546148,-30.2083455155492,17.2845772407366));
#4712=CARTESIAN_POINT('Ctrl Pts',(3.37094068270095,-29.6898924273955,17.2273043052763));
#4713=CARTESIAN_POINT('Ctrl Pts',(4.01431528178035,-28.4885418055165,17.1127136336125));
#4714=CARTESIAN_POINT('Ctrl Pts',(4.18547814755316,-27.8061836720571,17.0554409812454));
#4715=CARTESIAN_POINT('Ctrl Pts',(4.18663754642286,-26.4363906879155,16.9408495931827));
#4716=CARTESIAN_POINT('Ctrl Pts',(4.0150884896742,-25.7504104196397,16.8835772197774));
#4717=CARTESIAN_POINT('Ctrl Pts',(3.36714801944677,-24.5356000655517,16.7689851273202));
#4718=CARTESIAN_POINT('Ctrl Pts',(2.89009172502227,-24.0087892511978,16.7117130288065));
#4719=CARTESIAN_POINT('Ctrl Pts',(1.7402086697919,-23.2389101700822,16.5971202437039));
#4720=CARTESIAN_POINT('Ctrl Pts',(1.06776209555002,-22.9979372337308,16.5398484160816));
#4721=CARTESIAN_POINT('Ctrl Pts',(-0.31623274086958,-22.8602643582168,16.4252549498493));
#4722=CARTESIAN_POINT('Ctrl Pts',(-1.02644456351773,-22.9652272065363,16.3679833891743));
#4723=CARTESIAN_POINT('Ctrl Pts',(-2.31841804031954,-23.4988447092972,16.2533892531115));
#4724=CARTESIAN_POINT('Ctrl Pts',(-2.8982081868341,-23.9283243595328,16.1961179554988));
#4725=CARTESIAN_POINT('Ctrl Pts',(-3.79057690805528,-25.0133430809505,16.0815231606726));
#4726=CARTESIAN_POINT('Ctrl Pts',(-4.10102526300207,-25.6686660718134,16.024252122308));
#4727=CARTESIAN_POINT('Ctrl Pts',(-4.37797862822859,-27.0530885949626,15.909656679556));
#4728=CARTESIAN_POINT('Ctrl Pts',(-4.34271119481323,-27.7809795875592,15.8523858966855));
#4729=CARTESIAN_POINT('Ctrl Pts',(-3.93237495733071,-29.1392105157473,15.7377898166423));
#4730=CARTESIAN_POINT('Ctrl Pts',(-3.55632299466167,-29.7676390000464,15.6805192855666));
#4731=CARTESIAN_POINT('Ctrl Pts',(-2.54926136464863,-30.7770591329649,15.5659225786565));
#4732=CARTESIAN_POINT('Ctrl Pts',(-1.91829944896927,-31.1558975036044,15.5086522957306));
#4733=CARTESIAN_POINT('Ctrl Pts',(-0.547625232561448,-31.5734932671083,
15.3940549721839));
#4734=CARTESIAN_POINT('Ctrl Pts',(0.191015893047531,-31.6103769951178,15.3367849338207));
#4735=CARTESIAN_POINT('Ctrl Pts',(1.60357971999462,-31.3312243440256,15.222187003658));
#4736=CARTESIAN_POINT('Ctrl Pts',(2.27566348949658,-31.0140495365735,15.1649172063298));
#4737=CARTESIAN_POINT('Ctrl Pts',(3.39529563646339,-30.0975823003571,15.0503186793825));
#4738=CARTESIAN_POINT('Ctrl Pts',(3.84068011604263,-29.498165831456,14.9930491196166));
#4739=CARTESIAN_POINT('Ctrl Pts',(4.39882341638518,-28.1556730779471,14.8784500055221));
#4740=CARTESIAN_POINT('Ctrl Pts',(4.50961669585736,-27.4135215250066,14.8211806798972));
#4741=CARTESIAN_POINT('Ctrl Pts',(4.36838003559756,-25.9594643878227,14.706580988118));
#4742=CARTESIAN_POINT('Ctrl Pts',(4.11506029041641,-25.249312658991,14.64931189327));
#4743=CARTESIAN_POINT('Ctrl Pts',(3.30121940653211,-24.0276707334375,14.5347116330704));
#4744=CARTESIAN_POINT('Ctrl Pts',(2.74039982125199,-23.5183420501783,14.4774427656859));
#4745=CARTESIAN_POINT('Ctrl Pts',(1.44062797695419,-22.8212395033473,14.3628419461743));
#4746=CARTESIAN_POINT('Ctrl Pts',(0.702445412717409,-22.6355127980759,14.3055733029845));
#4747=CARTESIAN_POINT('Ctrl Pts',(-0.779466818671152,-22.6333745501127,
14.1909719330902));
#4748=CARTESIAN_POINT('Ctrl Pts',(-1.52154027083034,-22.8183992461163,14.133703510881));
#4749=CARTESIAN_POINT('Ctrl Pts',(-2.83568124304263,-23.5183337811168,14.0191015993632));
#4750=CARTESIAN_POINT('Ctrl Pts',(-3.40560315083273,-24.0337181522913,13.961833394971));
#4751=CARTESIAN_POINT('Ctrl Pts',(-4.23856228598614,-25.2762788645662,13.8472309504247));
#4752=CARTESIAN_POINT('Ctrl Pts',(-4.49948190557238,-26.0028485522343,13.789962960732));
#4753=CARTESIAN_POINT('Ctrl Pts',(-4.6490886604143,-27.4983069550493,13.6753599915962));
#4754=CARTESIAN_POINT('Ctrl Pts',(-4.53619916170288,-28.2656495705488,13.6180922135344));
#4755=CARTESIAN_POINT('Ctrl Pts',(-3.96055736820013,-29.661540425932,13.5034887280845));
#4756=CARTESIAN_POINT('Ctrl Pts',(-3.49715379610915,-30.2879729181394,13.4462211586326));
#4757=CARTESIAN_POINT('Ctrl Pts',(-2.32608670582391,-31.2521669466145,13.3316171649959));
#4758=CARTESIAN_POINT('Ctrl Pts',(-1.61885949052411,-31.5877524818146,13.2743498011764));
#4759=CARTESIAN_POINT('Ctrl Pts',(-0.124696310905245,-31.8874771910156,
13.1597453073302));
#4760=CARTESIAN_POINT('Ctrl Pts',(0.660815950487942,-31.8499065009576,13.1024781462114));
#4761=CARTESIAN_POINT('Ctrl Pts',(2.12655441499977,-31.4079152525417,12.9878731599857));
#4762=CARTESIAN_POINT('Ctrl Pts',(2.80470906709709,-31.0026671109796,12.9306061986817));
#4763=CARTESIAN_POINT('Ctrl Pts',(3.89400923429049,-29.9170086021089,12.8160007277616));
#4764=CARTESIAN_POINT('Ctrl Pts',(4.30293326762064,-29.2368576811396,12.7587339634332));
#4765=CARTESIAN_POINT('Ctrl Pts',(4.7539165316201,-27.7592163768989,12.6441280153592));
#4766=CARTESIAN_POINT('Ctrl Pts',(4.79414098254103,-26.9630153236094,12.5868614452008));
#4767=CARTESIAN_POINT('Ctrl Pts',(4.49400280036036,-25.4403847040206,12.4722550273998));
#4768=CARTESIAN_POINT('Ctrl Pts',(4.15263788850493,-24.7159678807397,12.4149886486516));
#4769=CARTESIAN_POINT('Ctrl Pts',(3.16577605609634,-23.509168568218,12.3003817683865));
#4770=CARTESIAN_POINT('Ctrl Pts',(2.52035612956819,-23.0290393182234,12.2431155783337));
#4771=CARTESIAN_POINT('Ctrl Pts',(1.07469387470518,-22.4272153063553,12.1285082427589));
#4772=CARTESIAN_POINT('Ctrl Pts',(0.275594950052222,-22.3074707664612,12.0712422387231));
#4773=CARTESIAN_POINT('Ctrl Pts',(-1.84866925673703,-22.5128307999096,11.915740909639));
#4774=CARTESIAN_POINT('Ctrl Pts',(-3.12603843365803,-23.2394090136764,11.8175868796768));
#4775=CARTESIAN_POINT('Ctrl Pts',(-4.3320981071104,-24.8804056714019,11.6703283443192));
#4776=CARTESIAN_POINT('Ctrl Pts',(-4.61674384788206,-25.5146057311216,11.6212316068295));
#4777=CARTESIAN_POINT('Ctrl Pts',(-4.83246869871424,-26.5137556598953,11.5476071541803));
#4778=CARTESIAN_POINT('Ctrl Pts',(-4.86977624768409,-26.8545749239038,11.5230638633071));
#4779=CARTESIAN_POINT('Ctrl Pts',(-4.87146626433893,-27.5373932865771,11.4739653075255));
#4780=CARTESIAN_POINT('Ctrl Pts',(-4.84802535953691,-27.8775521427343,11.449426192242));
#4781=CARTESIAN_POINT('Ctrl Pts',(-4.83316291400662,-28.2179621014742,11.4248820703399));
#4782=CARTESIAN_POINT('Ctrl Pts',(-3.4999738703761,-27.2127229078506,22.4975165797347));
#4783=CARTESIAN_POINT('Ctrl Pts',(-3.49925167603735,-27.7853247308279,22.440232944449));
#4784=CARTESIAN_POINT('Ctrl Pts',(-3.35443660091437,-28.3588149144678,22.3829524301632));
#4785=CARTESIAN_POINT('Ctrl Pts',(-2.53806849928542,-29.8821040197979,22.2111092380756));
#4786=CARTESIAN_POINT('Ctrl Pts',(-1.46144078073265,-30.6017196666142,22.0965431306844));
#4787=CARTESIAN_POINT('Ctrl Pts',(0.859996801537081,-30.8281850765549,21.8674140111125));
#4788=CARTESIAN_POINT('Ctrl Pts',(2.07105852363703,-30.3269992526889,21.7528496283989));
#4789=CARTESIAN_POINT('Ctrl Pts',(3.56718981158329,-28.5011078101942,21.5237158269035));
#4790=CARTESIAN_POINT('Ctrl Pts',(3.82657179215288,-27.2003590887291,21.4091531168235));
#4791=CARTESIAN_POINT('Ctrl Pts',(3.13178000345364,-24.9149626050602,21.1800148065395));
#4792=CARTESIAN_POINT('Ctrl Pts',(2.18341087092642,-23.965396720214,21.0654537187747));
#4793=CARTESIAN_POINT('Ctrl Pts',(-0.129624685393233,-23.2649124957247,
20.8363110649486));
#4794=CARTESIAN_POINT('Ctrl Pts',(-1.46146638375645,-23.5287584813108,20.7217515508348));
#4795=CARTESIAN_POINT('Ctrl Pts',(-3.35088189452712,-25.0803749934778,20.4926047112563));
#4796=CARTESIAN_POINT('Ctrl Pts',(-3.87762063512896,-26.3487540133528,20.3780467237371));
#4797=CARTESIAN_POINT('Ctrl Pts',(-3.63477320284824,-28.8097653712122,20.1488958491381));
#4798=CARTESIAN_POINT('Ctrl Pts',(-2.86425015889221,-29.9655506417163,20.0343393426895));
#4799=CARTESIAN_POINT('Ctrl Pts',(-0.658456006019151,-31.1444163926324,
19.8051845771816));
#4800=CARTESIAN_POINT('Ctrl Pts',(0.746297759417265,-31.1460633761619,19.690629507766));
#4801=CARTESIAN_POINT('Ctrl Pts',(2.97687510367843,-29.9539934454761,19.4614709891321));
#4802=CARTESIAN_POINT('Ctrl Pts',(3.76754784711476,-28.7739735063694,19.3469173141651));
#4803=CARTESIAN_POINT('Ctrl Pts',(4.01867655925237,-26.2291263727762,19.1177551742263));
#4804=CARTESIAN_POINT('Ctrl Pts',(3.47097521400111,-24.9015751449147,19.0032028524946));
#4805=CARTESIAN_POINT('Ctrl Pts',(1.4730218826762,-23.260888053339,18.7740372174575));
#4806=CARTESIAN_POINT('Ctrl Pts',(0.0495870334641008,-22.9755028102541,
18.6594862090688));
#4807=CARTESIAN_POINT('Ctrl Pts',(-2.45154148772098,-23.733090471763,18.4303171997907));
#4808=CARTESIAN_POINT('Ctrl Pts',(-3.49085030038139,-24.7690320660619,18.3157674661644));
#4809=CARTESIAN_POINT('Ctrl Pts',(-4.25891245790086,-27.2963085987281,18.086595198388));
#4810=CARTESIAN_POINT('Ctrl Pts',(-3.97208283893911,-28.7513950463358,17.9720467021754));
#4811=CARTESIAN_POINT('Ctrl Pts',(-2.27985892683281,-30.8159626032593,17.7428712868959));
#4812=CARTESIAN_POINT('Ctrl Pts',(-0.896242888528564,-31.3920251821923,
17.6283239919319));
#4813=CARTESIAN_POINT('Ctrl Pts',(1.11729729633126,-31.1951529721948,17.4564401496407));
#4814=CARTESIAN_POINT('Ctrl Pts',(1.77293266626044,-30.9607296662042,17.3991669448048));
#4815=CARTESIAN_POINT('Ctrl Pts',(2.90078714764444,-30.2083552754577,17.2845769755984));
#4816=CARTESIAN_POINT('Ctrl Pts',(3.37095107897927,-29.6899006325071,17.2273040579683));
#4817=CARTESIAN_POINT('Ctrl Pts',(4.01432777756716,-28.4885461927946,17.1127133602641));
#4818=CARTESIAN_POINT('Ctrl Pts',(4.18549118397379,-27.8061860074247,17.0554407256377));
#4819=CARTESIAN_POINT('Ctrl Pts',(4.18665063468174,-26.4363886665888,16.9408493116638));
#4820=CARTESIAN_POINT('Ctrl Pts',(4.01510108746783,-25.7504063338809,16.8835769559103));
#4821=CARTESIAN_POINT('Ctrl Pts',(3.36715860920047,-24.5355921131514,16.7689848376699));
#4822=CARTESIAN_POINT('Ctrl Pts',(2.89010090908047,-24.0087797093735,16.71171275672));
#4823=CARTESIAN_POINT('Ctrl Pts',(1.74021426019986,-23.2388981648313,16.5971199459608));
#4824=CARTESIAN_POINT('Ctrl Pts',(1.06776569703458,-22.9979244893974,16.5398481358153));
#4825=CARTESIAN_POINT('Ctrl Pts',(-0.316233469917037,-22.8602511354241,
16.4252546440519));
#4826=CARTESIAN_POINT('Ctrl Pts',(-1.02644739499413,-22.9652142695065,16.3679831007674));
#4827=CARTESIAN_POINT('Ctrl Pts',(-2.31842491646956,-23.4988333917331,16.2533889392978));
#4828=CARTESIAN_POINT('Ctrl Pts',(-2.89821678241042,-23.9283142850487,16.1961176589903));
#4829=CARTESIAN_POINT('Ctrl Pts',(-3.79058830723667,-25.0133363413519,16.0815228388804));
#4830=CARTESIAN_POINT('Ctrl Pts',(-4.10103759256865,-25.6686612390088,16.0242518177364));
#4831=CARTESIAN_POINT('Ctrl Pts',(-4.37799185824023,-27.0530880248399,15.9096563498227));
#4832=CARTESIAN_POINT('Ctrl Pts',(-4.34272434648572,-27.7809811376122,15.852385584089));
#4833=CARTESIAN_POINT('Ctrl Pts',(-3.93238689367438,-29.1392162495564,15.7377894790049));
#4834=CARTESIAN_POINT('Ctrl Pts',(-3.5563338624862,-29.7676465667086,15.680518964983));
#4835=CARTESIAN_POINT('Ctrl Pts',(-2.54926918843734,-30.7770698163966,15.5659222331516));
#4836=CARTESIAN_POINT('Ctrl Pts',(-1.91830546644135,-31.155909299737,15.5086519671974));
#4837=CARTESIAN_POINT('Ctrl Pts',(-0.547627096231643,-31.5735063769721,
15.394054618848));
#4838=CARTESIAN_POINT('Ctrl Pts',(0.191016146883062,-31.6103902347893,15.3367845973752));
#4839=CARTESIAN_POINT('Ctrl Pts',(1.60358425638348,-31.3312367841738,15.2221866425272));
#4840=CARTESIAN_POINT('Ctrl Pts',(2.27566995450071,-31.0140610930252,15.1649168620087));
#4841=CARTESIAN_POINT('Ctrl Pts',(3.39530550137407,-30.0975911329029,15.0503183104925));
#4842=CARTESIAN_POINT('Ctrl Pts',(3.84069126522877,-29.4981729755389,14.9930487674564));
#4843=CARTESIAN_POINT('Ctrl Pts',(4.39883627990966,-28.1556762170847,14.8784496289083));
#4844=CARTESIAN_POINT('Ctrl Pts',(4.50962989605486,-27.4135225696958,14.8211803199342));
#4845=CARTESIAN_POINT('Ctrl Pts',(4.36839285973953,-25.9594610923935,14.7065806038156));
#4846=CARTESIAN_POINT('Ctrl Pts',(4.11507242416446,-25.2493073577679,14.6493115255399));
#4847=CARTESIAN_POINT('Ctrl Pts',(3.30122916269765,-24.0276617819218,14.5347112411141));
#4848=CARTESIAN_POINT('Ctrl Pts',(2.7404080230466,-23.5183316552038,14.4774423902243));
#4849=CARTESIAN_POINT('Ctrl Pts',(1.44063236119846,-22.8212270099635,14.3628415465987));
#4850=CARTESIAN_POINT('Ctrl Pts',(0.70244774573194,-22.6354997644271,14.3055729198267));
#4851=CARTESIAN_POINT('Ctrl Pts',(-0.779468841558015,-22.6333614654686,
14.1909715259295));
#4852=CARTESIAN_POINT('Ctrl Pts',(-1.52154435736691,-22.8183866519466,14.1337031200619));
#4853=CARTESIAN_POINT('Ctrl Pts',(-2.83568919509919,-23.5183231953511,14.0191011846514));
#4854=CARTESIAN_POINT('Ctrl Pts',(-3.40561269160967,-24.0337089718608,13.9618329965252));
#4855=CARTESIAN_POINT('Ctrl Pts',(-4.2385742890103,-25.2762732775619,13.8472305281954));
#4856=CARTESIAN_POINT('Ctrl Pts',(-4.49949464722015,-26.0028449534998,13.7899625546938));
#4857=CARTESIAN_POINT('Ctrl Pts',(-4.64910187957824,-27.4983076860702,13.6753595618827));
#4858=CARTESIAN_POINT('Ctrl Pts',(-4.53621209500216,-28.2656524031987,13.6180917999378));
#4859=CARTESIAN_POINT('Ctrl Pts',(-3.96056868157127,-29.661547302102,13.5034882909199));
#4860=CARTESIAN_POINT('Ctrl Pts',(-3.49716386668666,-30.2879815129736,13.4462207375114));
#4861=CARTESIAN_POINT('Ctrl Pts',(-2.32609344166591,-31.2521783437993,13.3316167204129));
#4862=CARTESIAN_POINT('Ctrl Pts',(-1.61886432018724,-31.5877648088394,13.274349372564));
#4863=CARTESIAN_POINT('Ctrl Pts',(-0.124696878631275,-31.88749041744,13.1597448553615));
#4864=CARTESIAN_POINT('Ctrl Pts',(0.66081750213183,-31.8499196488467,13.1024777101411));
#4865=CARTESIAN_POINT('Ctrl Pts',(2.12656014922713,-31.4079271845322,12.9878727006634));
#4866=CARTESIAN_POINT('Ctrl Pts',(2.80471663336618,-31.0026779746561,12.9306057551862));
#4867=CARTESIAN_POINT('Ctrl Pts',(3.89401991600716,-29.9170164218118,12.8160002611176));
#4868=CARTESIAN_POINT('Ctrl Pts',(4.30294506141158,-29.2368636950917,12.7587335125451));
#4869=CARTESIAN_POINT('Ctrl Pts',(4.75392963799469,-27.7592182377462,12.6441275414253));
#4870=CARTESIAN_POINT('Ctrl Pts',(4.79415421843191,-26.9630150677512,12.5868609869525));
#4871=CARTESIAN_POINT('Ctrl Pts',(4.49401523604375,-25.4403801667867,12.4722545462074));
#4872=CARTESIAN_POINT('Ctrl Pts',(4.15264944060989,-24.7159614157411,12.4149881830751));
#4873=CARTESIAN_POINT('Ctrl Pts',(3.16578488425683,-23.5091587046932,12.3003812799668));
#4874=CARTESIAN_POINT('Ctrl Pts',(2.52036326977255,-23.029028171125,12.2431151054609));
#4875=CARTESIAN_POINT('Ctrl Pts',(1.07469701059825,-22.4272024461661,12.1285077471428));
#4876=CARTESIAN_POINT('Ctrl Pts',(0.275595992279665,-22.3074575699848,12.0712417585854));
#4877=CARTESIAN_POINT('Ctrl Pts',(-1.84867410165387,-22.5128181147607,11.9157403987775));
#4878=CARTESIAN_POINT('Ctrl Pts',(-3.126046686507,-23.239398259682,11.8175863798246));
#4879=CARTESIAN_POINT('Ctrl Pts',(-4.33210964259808,-24.8803992898634,11.6703278427641));
#4880=CARTESIAN_POINT('Ctrl Pts',(-4.61675618009252,-25.5146010763329,11.6212310968322));
#4881=CARTESIAN_POINT('Ctrl Pts',(-4.83248163235518,-26.5137536581576,11.5476066464927));
#4882=CARTESIAN_POINT('Ctrl Pts',(-4.86978929142209,-26.8545738310615,11.5230633554386));
#4883=CARTESIAN_POINT('Ctrl Pts',(-4.87147933058113,-27.5373940588702,11.473964789632));
#4884=CARTESIAN_POINT('Ctrl Pts',(-4.84803840451156,-27.877552675042,11.4494256757284));
#4885=CARTESIAN_POINT('Ctrl Pts',(-4.83317595898128,-28.217962633782,11.4248815538263));
#4886=CARTESIAN_POINT('Ctrl Pts',(-3.4999869352734,-27.2127227490105,22.4975165961398));
#4887=CARTESIAN_POINT('Ctrl Pts',(-3.49926476744378,-27.7853267509384,22.4402329465374));
#4888=CARTESIAN_POINT('Ctrl Pts',(-3.35444920153117,-28.3588189994771,22.3829524521897));
#4889=CARTESIAN_POINT('Ctrl Pts',(-2.53807808935145,-29.8821139057597,22.2111092142027));
#4890=CARTESIAN_POINT('Ctrl Pts',(-1.46144655006658,-30.6017321733,22.0965431484635));
#4891=CARTESIAN_POINT('Ctrl Pts',(0.859999693521789,-30.8281985427089,21.867413968396));
#4892=CARTESIAN_POINT('Ctrl Pts',(2.07106571728588,-30.3270109980947,21.7528496268498));
#4893=CARTESIAN_POINT('Ctrl Pts',(3.56720261496358,-28.5011128868879,21.5237157655468));
#4894=CARTESIAN_POINT('Ctrl Pts',(3.82658555467438,-27.2003596328324,21.4091530961607));
#4895=CARTESIAN_POINT('Ctrl Pts',(3.1317913376183,-24.9149547798571,21.180014726742));
#4896=CARTESIAN_POINT('Ctrl Pts',(2.18341896934776,-23.9653855794009,21.0654536792084));
#4897=CARTESIAN_POINT('Ctrl Pts',(-0.129624895009774,-23.2648987243724,
20.8363109669058));
#4898=CARTESIAN_POINT('Ctrl Pts',(-1.46147114777366,-23.5287455582848,20.7217514925706));
#4899=CARTESIAN_POINT('Ctrl Pts',(-3.35089346140745,-25.0803675170051,20.4926045951597));
#4900=CARTESIAN_POINT('Ctrl Pts',(-3.87763402690497,-26.3487507949125,20.3780466469766));
#4901=CARTESIAN_POINT('Ctrl Pts',(-3.63478584531403,-28.8097708350949,20.1488957151756));
#4902=CARTESIAN_POINT('Ctrl Pts',(-2.86426027486676,-29.9655599884758,20.0343392476302));
#4903=CARTESIAN_POINT('Ctrl Pts',(-0.658458486544607,-31.1444299398784,
19.8051844255374));
#4904=CARTESIAN_POINT('Ctrl Pts',(0.746299910894372,-31.1460769799159,19.6906293946012));
#4905=CARTESIAN_POINT('Ctrl Pts',(2.97688498967388,-29.9540030341285,19.4614708199869));
#4906=CARTESIAN_POINT('Ctrl Pts',(3.76756035341267,-28.7739792751586,19.3469171830846));
#4907=CARTESIAN_POINT('Ctrl Pts',(4.01869002402406,-26.2291234798987,19.1177549877571));
#4908=CARTESIAN_POINT('Ctrl Pts',(3.47098695847717,-24.9015679512733,19.0032027036843));
#4909=CARTESIAN_POINT('Ctrl Pts',(1.47302695767718,-23.2608752507521,18.7740370138381));
#4910=CARTESIAN_POINT('Ctrl Pts',(0.0495875769098387,-22.9754890487136,
18.6594860427109));
#4911=CARTESIAN_POINT('Ctrl Pts',(-2.45154931318775,-23.733079139667,18.4303169791917));
#4912=CARTESIAN_POINT('Ctrl Pts',(-3.49086144065754,-24.7690239689578,18.3157672824377));
#4913=CARTESIAN_POINT('Ctrl Pts',(-4.25892622749306,-27.2963088098151,18.0865949609766));
#4914=CARTESIAN_POINT('Ctrl Pts',(-3.97209576034448,-28.7513998106872,17.9720465012551));
#4915=CARTESIAN_POINT('Ctrl Pts',(-2.27986640092468,-30.8159741693962,17.7428710328365));
#4916=CARTESIAN_POINT('Ctrl Pts',(-0.896246105632028,-31.3920385726492,
17.6283237739899));
#4917=CARTESIAN_POINT('Ctrl Pts',(1.11730059050837,-31.1951657997167,17.4564398922454));
#4918=CARTESIAN_POINT('Ctrl Pts',(1.77293796695974,-30.9607418032691,17.3991667053302));
#4919=CARTESIAN_POINT('Ctrl Pts',(2.90079609967118,-30.2083650352605,17.2845767099533));
#4920=CARTESIAN_POINT('Ctrl Pts',(3.37096147508705,-29.6899088375397,17.2273038101533));
#4921=CARTESIAN_POINT('Ctrl Pts',(4.01434027316612,-28.4885505800527,17.1127130864091));
#4922=CARTESIAN_POINT('Ctrl Pts',(4.18550422020648,-27.8061883428027,17.0554404695231));
#4923=CARTESIAN_POINT('Ctrl Pts',(4.18666372276521,-26.4363866453329,16.9408490296383));
#4924=CARTESIAN_POINT('Ctrl Pts',(4.01511368510023,-25.7504022482198,16.8835766915364));
#4925=CARTESIAN_POINT('Ctrl Pts',(3.36716919883249,-24.5355841608964,16.768984547513));
#4926=CARTESIAN_POINT('Ctrl Pts',(2.89011009304215,-24.0087701677114,16.7117124841267));
#4927=CARTESIAN_POINT('Ctrl Pts',(1.74021985056861,-23.238886159766,16.5971196477113));
#4928=CARTESIAN_POINT('Ctrl Pts',(1.06776929851019,-22.9979117452528,16.5398478550424));
#4929=CARTESIAN_POINT('Ctrl Pts',(-0.316234198911765,-22.8602379128138,
16.4252543377482));
#4930=CARTESIAN_POINT('Ctrl Pts',(-1.02645022638954,-22.9652013326477,16.367982811854));
#4931=CARTESIAN_POINT('Ctrl Pts',(-2.31843179248706,-23.4988220743056,16.253388624978));
#4932=CARTESIAN_POINT('Ctrl Pts',(-2.89822537783462,-23.9283042106777,16.1961173619753));
#4933=CARTESIAN_POINT('Ctrl Pts',(-3.7905997062367,-25.0133296018116,16.0815225165821));
#4934=CARTESIAN_POINT('Ctrl Pts',(-4.10104992194752,-25.6686564062324,16.0242515126585));
#4935=CARTESIAN_POINT('Ctrl Pts',(-4.37800508806418,-27.0530874546831,15.9096560195834));
#4936=CARTESIAN_POINT('Ctrl Pts',(-4.34273749797898,-27.7809826876019,15.8523852709862));
#4937=CARTESIAN_POINT('Ctrl Pts',(-3.93239882986814,-29.1392219832472,15.7377891408615));
#4938=CARTESIAN_POINT('Ctrl Pts',(-3.55634473018214,-29.7676541332304,15.6805186438933));
#4939=CARTESIAN_POINT('Ctrl Pts',(-2.5492770121493,-30.7770804996531,15.5659218871409));
#4940=CARTESIAN_POINT('Ctrl Pts',(-1.91831148386587,-31.1559210956849,15.5086516381582));
#4941=CARTESIAN_POINT('Ctrl Pts',(-0.547628959916488,-31.573519486645,15.3940542650064));
#4942=CARTESIAN_POINT('Ctrl Pts',(0.191016400673711,-31.6104034742754,15.3367842604237));
#4943=CARTESIAN_POINT('Ctrl Pts',(1.60358879266949,-31.3312492241601,15.2221862808907));
#4944=CARTESIAN_POINT('Ctrl Pts',(2.27567641937781,-31.0140726493341,15.1649165171817));
#4945=CARTESIAN_POINT('Ctrl Pts',(3.39531536611764,-30.0975999653541,15.0503179410969));
#4946=CARTESIAN_POINT('Ctrl Pts',(3.84070241423541,-29.4981801195554,14.9930484147904));
#4947=CARTESIAN_POINT('Ctrl Pts',(4.39884914324192,-28.1556793562174,14.8784492517891));
#4948=CARTESIAN_POINT('Ctrl Pts',(4.50964309606246,-27.4135236144109,14.8211799594654));
#4949=CARTESIAN_POINT('Ctrl Pts',(4.36840568370932,-25.9594577970506,14.7065802190078));
#4950=CARTESIAN_POINT('Ctrl Pts',(4.11508455775685,-25.249302056657,14.6493111573042));
#4951=CARTESIAN_POINT('Ctrl Pts',(3.30123891875162,-24.0276528305633,14.5347108486526));
#4952=CARTESIAN_POINT('Ctrl Pts',(2.74041622475651,-23.5183212604017,14.4774420142573));
#4953=CARTESIAN_POINT('Ctrl Pts',(1.44063674541817,-22.8212145167712,14.3628411465179));
#4954=CARTESIAN_POINT('Ctrl Pts',(0.702450078752852,-22.6354867309707,14.3055725361634));
#4955=CARTESIAN_POINT('Ctrl Pts',(-0.779470864376416,-22.6333483810052,
14.1909711182638));
#4956=CARTESIAN_POINT('Ctrl Pts',(-1.52154844380728,-22.818374057944,14.1337027287374));
#4957=CARTESIAN_POINT('Ctrl Pts',(-2.83569714701013,-23.5183126097129,14.0191007694346));
#4958=CARTESIAN_POINT('Ctrl Pts',(-3.40562223222298,-24.0336997915325,13.9618325975741));
#4959=CARTESIAN_POINT('Ctrl Pts',(-4.23858629184574,-25.2762676906016,13.8472301054612));
#4960=CARTESIAN_POINT('Ctrl Pts',(-4.49950738867518,-26.0028413547787,13.7899621481505));
#4961=CARTESIAN_POINT('Ctrl Pts',(-4.64911509855466,-27.4983084170412,13.6753591316644));
#4962=CARTESIAN_POINT('Ctrl Pts',(-4.53622502812489,-28.2656552357695,13.6180913858362));
#4963=CARTESIAN_POINT('Ctrl Pts',(-3.96057999480023,-29.6615541781397,13.5034878532506));
#4964=CARTESIAN_POINT('Ctrl Pts',(-3.49717393714537,-30.2879901076548,13.4462203158853));
#4965=CARTESIAN_POINT('Ctrl Pts',(-2.32610017744464,-31.2521897408003,13.3316162753254));
#4966=CARTESIAN_POINT('Ctrl Pts',(-1.61886914981746,-31.5877771356732,13.2743489434468));
#4967=CARTESIAN_POINT('Ctrl Pts',(-0.124697446388046,-31.8875036436721,
13.1597444028882));
#4968=CARTESIAN_POINT('Ctrl Pts',(0.660819053714784,-31.8499327965513,13.1024772735659));
#4969=CARTESIAN_POINT('Ctrl Pts',(2.12656588333675,-31.4079391163672,12.9878722408366));
#4970=CARTESIAN_POINT('Ctrl Pts',(2.80472419949459,-31.0026888381985,12.930605311186));
#4971=CARTESIAN_POINT('Ctrl Pts',(3.89403059754656,-29.9170242414328,12.8159997939693));
#4972=CARTESIAN_POINT('Ctrl Pts',(4.302956855015,-29.2368697089914,12.7587330611525));
#4973=CARTESIAN_POINT('Ctrl Pts',(4.75394274417405,-27.7592200986048,12.6441270669872));
#4974=CARTESIAN_POINT('Ctrl Pts',(4.79416745413243,-26.963014811935,12.5868605281998));
#4975=CARTESIAN_POINT('Ctrl Pts',(4.49402767155989,-25.4403756296546,12.4722540645109));
#4976=CARTESIAN_POINT('Ctrl Pts',(4.15266099256647,-24.7159549508694,12.4149877169943));
#4977=CARTESIAN_POINT('Ctrl Pts',(3.16579371231746,-23.509148841337,12.300380791043));
#4978=CARTESIAN_POINT('Ctrl Pts',(2.52037040990553,-23.0290170242085,12.2431146320838));
#4979=CARTESIAN_POINT('Ctrl Pts',(1.07470014648255,-22.427189586173,12.1285072510228));
#4980=CARTESIAN_POINT('Ctrl Pts',(0.275597034529758,-22.3074443737027,12.0712412779435));
#4981=CARTESIAN_POINT('Ctrl Pts',(-1.84867894646398,-22.5128054297831,11.9157398874122));
#4982=CARTESIAN_POINT('Ctrl Pts',(-3.12605493920518,-23.2393875058207,11.8175858794686));
#4983=CARTESIAN_POINT('Ctrl Pts',(-4.33212117789959,-24.8803929083851,11.670327340705));
#4984=CARTESIAN_POINT('Ctrl Pts',(-4.61676851210983,-25.5145964215772,11.621230586331));
#4985=CARTESIAN_POINT('Ctrl Pts',(-4.83249456580181,-26.5137516564125,11.5476061383012));
#4986=CARTESIAN_POINT('Ctrl Pts',(-4.86980233496674,-26.8545727381983,11.5230628470662));
#4987=CARTESIAN_POINT('Ctrl Pts',(-4.87149239663453,-27.5373948311151,11.4739642712348));
#4988=CARTESIAN_POINT('Ctrl Pts',(-4.8480514492971,-27.8775532073051,11.4494251587111));
#4989=CARTESIAN_POINT('Ctrl Pts',(-4.83318900376681,-28.2179631660451,11.424881036809));
#4990=CARTESIAN_POINT('Ctrl Pts',(-3.5,-27.2127225901214,22.4975166120351));
#4991=CARTESIAN_POINT('Ctrl Pts',(-3.49927785868713,-27.7853287709716,22.4402329481162));
#4992=CARTESIAN_POINT('Ctrl Pts',(-3.35446180200001,-28.3588230843844,22.3829524737063));
#4993=CARTESIAN_POINT('Ctrl Pts',(-2.53808767932955,-29.8821237915549,22.2111091898206));
#4994=CARTESIAN_POINT('Ctrl Pts',(-1.46145231937317,-30.6017446798008,22.0965431657326));
#4995=CARTESIAN_POINT('Ctrl Pts',(0.860002585417323,-30.8282120086964,21.8674139251703));
#4996=CARTESIAN_POINT('Ctrl Pts',(2.07107291079633,-30.3270227433741,21.752849624791));
#4997=CARTESIAN_POINT('Ctrl Pts',(3.56721541815537,-28.5011179635623,21.5237157036811));
#4998=CARTESIAN_POINT('Ctrl Pts',(3.82659931701312,-27.20036017698,21.4091530749885));
#4999=CARTESIAN_POINT('Ctrl Pts',(3.13180267166131,-24.9149469548,21.1800146464357));
#5000=CARTESIAN_POINT('Ctrl Pts',(2.18342706770339,-23.9653744387647,21.0654536391327));
#5001=CARTESIAN_POINT('Ctrl Pts',(-0.129625104573071,-23.2648849532031,
20.8363108683544));
#5002=CARTESIAN_POINT('Ctrl Pts',(-1.46147591168062,-23.5287326354126,20.7217514337973));
#5003=CARTESIAN_POINT('Ctrl Pts',(-3.35090502810569,-25.0803600405907,20.4926044785548));
#5004=CARTESIAN_POINT('Ctrl Pts',(-3.87764741849126,-26.3487475764667,20.3780465697071));
#5005=CARTESIAN_POINT('Ctrl Pts',(-3.63479848762931,-28.8097762988588,20.148895580705));
#5006=CARTESIAN_POINT('Ctrl Pts',(-2.86427039073957,-29.9655693350743,20.0343391520621));
#5007=CARTESIAN_POINT('Ctrl Pts',(-0.65846096708456,-31.1444434869326,19.8051842733852));
#5008=CARTESIAN_POINT('Ctrl Pts',(0.74630206229462,-31.1460905834951,19.6906292809279));
#5009=CARTESIAN_POINT('Ctrl Pts',(2.97689487550167,-29.9540126226856,19.4614706503338));
#5010=CARTESIAN_POINT('Ctrl Pts',(3.76757285952208,-28.7739850439139,19.3469170514958));
#5011=CARTESIAN_POINT('Ctrl Pts',(4.0187034886225,-26.2291205871072,19.1177548007802));
#5012=CARTESIAN_POINT('Ctrl Pts',(3.47099870281935,-24.9015607577697,19.0032025543658));
#5013=CARTESIAN_POINT('Ctrl Pts',(1.47303203265274,-23.2608624483575,18.7740368097113));
#5014=CARTESIAN_POINT('Ctrl Pts',(0.0495881203952384,-22.9754752873616,
18.6594858758451));
#5015=CARTESIAN_POINT('Ctrl Pts',(-2.45155713850874,-23.7330678076998,18.4303167580854));
#5016=CARTESIAN_POINT('Ctrl Pts',(-3.49087258075457,-24.7690158719264,18.3157670982032));
#5017=CARTESIAN_POINT('Ctrl Pts',(-4.25893999689643,-27.296309020853,18.0865947230583));
#5018=CARTESIAN_POINT('Ctrl Pts',(-3.97210868158914,-28.7514045749302,17.9720462998272));
#5019=CARTESIAN_POINT('Ctrl Pts',(-2.27987387495177,-30.8159857353485,17.7428707782702));
#5020=CARTESIAN_POINT('Ctrl Pts',(-0.896249322735714,-31.3920519629118,
17.6283235555406));
#5021=CARTESIAN_POINT('Ctrl Pts',(1.11730388459739,-31.1951786270721,17.4564396343434));
#5022=CARTESIAN_POINT('Ctrl Pts',(1.77294326754581,-30.9607539401843,17.3991664653485));
#5023=CARTESIAN_POINT('Ctrl Pts',(2.90080505154166,-30.2083747949576,17.2845764438015));
#5024=CARTESIAN_POINT('Ctrl Pts',(3.37097187102428,-29.6899170424932,17.2273035618313));
#5025=CARTESIAN_POINT('Ctrl Pts',(4.01435276857721,-28.4885549672909,17.1127128120475));
#5026=CARTESIAN_POINT('Ctrl Pts',(4.18551725625119,-27.8061906781911,17.0554402129015));
#5027=CARTESIAN_POINT('Ctrl Pts',(4.18667681067326,-26.4363846241478,16.9408487471063));
#5028=CARTESIAN_POINT('Ctrl Pts',(4.01512628257138,-25.7503981626563,16.8835764266556));
#5029=CARTESIAN_POINT('Ctrl Pts',(3.3671797883428,-24.5355762087865,16.7689842568497));
#5030=CARTESIAN_POINT('Ctrl Pts',(2.89011927690729,-24.0087606262116,16.7117122110268));
#5031=CARTESIAN_POINT('Ctrl Pts',(1.74022544089816,-23.2388741548863,16.5971193489555));
#5032=CARTESIAN_POINT('Ctrl Pts',(1.06777289997686,-22.997899001297,16.5398475737628));
#5033=CARTESIAN_POINT('Ctrl Pts',(-0.316234927853767,-22.8602246903861,
16.4252540309383));
#5034=CARTESIAN_POINT('Ctrl Pts',(-1.02645305770396,-22.9651883959601,16.3679825224341));
#5035=CARTESIAN_POINT('Ctrl Pts',(-2.31843866837204,-23.4988107570144,16.253388310152));
#5036=CARTESIAN_POINT('Ctrl Pts',(-2.89823397310667,-23.9282941364198,16.196117064454));
#5037=CARTESIAN_POINT('Ctrl Pts',(-3.79061110505536,-25.0133228623296,16.0815221937778));
#5038=CARTESIAN_POINT('Ctrl Pts',(-4.10106225113868,-25.6686515734845,16.0242512070742));
#5039=CARTESIAN_POINT('Ctrl Pts',(-4.37801831770041,-27.0530868844925,15.909655688838));
#5040=CARTESIAN_POINT('Ctrl Pts',(-4.34275064929299,-27.7809842375283,15.8523849573772));
#5041=CARTESIAN_POINT('Ctrl Pts',(-3.93241076591198,-29.1392277168195,15.7377888022123));
#5042=CARTESIAN_POINT('Ctrl Pts',(-3.55635559774948,-29.7676616996119,15.6805183222975));
#5043=CARTESIAN_POINT('Ctrl Pts',(-2.5492848357845,-30.7770911827345,15.5659215406245));
#5044=CARTESIAN_POINT('Ctrl Pts',(-1.91831750124282,-31.1559328914483,15.508651308613));
#5045=CARTESIAN_POINT('Ctrl Pts',(-0.547630823615979,-31.573532596127,15.3940539106591));
#5046=CARTESIAN_POINT('Ctrl Pts',(0.191016654419482,-31.6104167135759,15.3367839229662));
#5047=CARTESIAN_POINT('Ctrl Pts',(1.60359332885263,-31.3312616639846,15.2221859187487));
#5048=CARTESIAN_POINT('Ctrl Pts',(2.27568288412789,-31.0140842055001,15.1649161718489));
#5049=CARTESIAN_POINT('Ctrl Pts',(3.39532523069409,-30.0976087977106,15.0503175711959));
#5050=CARTESIAN_POINT('Ctrl Pts',(3.84071356306253,-29.4981872635055,14.9930480616187));
#5051=CARTESIAN_POINT('Ctrl Pts',(4.39886200638194,-28.1556824953451,14.8784488741645));
#5052=CARTESIAN_POINT('Ctrl Pts',(4.50965629588013,-27.4135246591517,14.821179598491));
#5053=CARTESIAN_POINT('Ctrl Pts',(4.36841850750692,-25.9594545017938,14.7065798336947));
#5054=CARTESIAN_POINT('Ctrl Pts',(4.11509669119356,-25.2492967556584,14.649310788563));
#5055=CARTESIAN_POINT('Ctrl Pts',(3.301248674694,-24.027643879362,14.5347104556859));
#5056=CARTESIAN_POINT('Ctrl Pts',(2.7404244263817,-23.5183108657722,14.4774416377848));
#5057=CARTESIAN_POINT('Ctrl Pts',(1.44064112961331,-22.8212020237703,14.3628407459321));
#5058=CARTESIAN_POINT('Ctrl Pts',(0.702452411780137,-22.6354736977066,14.3055721519949));
#5059=CARTESIAN_POINT('Ctrl Pts',(-0.779472887126354,-22.6333352967227,
14.190970710093));
#5060=CARTESIAN_POINT('Ctrl Pts',(-1.52155253015143,-22.8183614641083,14.1337023369077));
#5061=CARTESIAN_POINT('Ctrl Pts',(-2.83570509877543,-23.5183020242021,14.0191003537129));
#5062=CARTESIAN_POINT('Ctrl Pts',(-3.40563177267265,-24.0336906113064,13.9618321981179));
#5063=CARTESIAN_POINT('Ctrl Pts',(-4.23859829449245,-25.2762621036854,13.8472296822221));
#5064=CARTESIAN_POINT('Ctrl Pts',(-4.49952012993745,-26.0028377560707,13.7899617411021));
#5065=CARTESIAN_POINT('Ctrl Pts',(-4.64912831734354,-27.4983091479623,13.6753587009413));
#5066=CARTESIAN_POINT('Ctrl Pts',(-4.53623796107103,-28.2656580682614,13.6180909712297));
#5067=CARTESIAN_POINT('Ctrl Pts',(-3.96059130788698,-29.6615610540449,13.5034874150766));
#5068=CARTESIAN_POINT('Ctrl Pts',(-3.49718400748527,-30.2879987021829,13.4462198937543));
#5069=CARTESIAN_POINT('Ctrl Pts',(-2.32610691316009,-31.2522011376172,13.3316158297333));
#5070=CARTESIAN_POINT('Ctrl Pts',(-1.61887397941475,-31.5877894623157,13.2743485138248));
#5071=CARTESIAN_POINT('Ctrl Pts',(-0.124698014175552,-31.8875168697119,
13.1597439499104));
#5072=CARTESIAN_POINT('Ctrl Pts',(0.660820605236803,-31.8499459440715,13.1024768364861));
#5073=CARTESIAN_POINT('Ctrl Pts',(2.12657161732859,-31.4079510480467,12.9878717805055));
#5074=CARTESIAN_POINT('Ctrl Pts',(2.8047317654823,-31.0026997016065,12.9306048666812));
#5075=CARTESIAN_POINT('Ctrl Pts',(3.89404127890867,-29.9170320609718,12.8159993263168));
#5076=CARTESIAN_POINT('Ctrl Pts',(4.30296864843086,-29.2368757228388,12.7587326092554));
#5077=CARTESIAN_POINT('Ctrl Pts',(4.75395585015817,-27.7592219594744,12.6441265920449));
#5078=CARTESIAN_POINT('Ctrl Pts',(4.79418068964257,-26.9630145561609,12.5868600689426));
#5079=CARTESIAN_POINT('Ctrl Pts',(4.49404010690874,-25.4403710926243,12.4722535823103));
#5080=CARTESIAN_POINT('Ctrl Pts',(4.15267254437464,-24.7159484861244,12.4149872504092));
#5081=CARTESIAN_POINT('Ctrl Pts',(3.16580254027823,-23.5091389781496,12.3003803016153));
#5082=CARTESIAN_POINT('Ctrl Pts',(2.52037754996715,-23.0290058774741,12.2431141582025));
#5083=CARTESIAN_POINT('Ctrl Pts',(1.07470328235808,-22.427176726376,12.1285067543989));
#5084=CARTESIAN_POINT('Ctrl Pts',(0.275598076802496,-22.3074311776151,12.0712407967975));
#5085=CARTESIAN_POINT('Ctrl Pts',(-1.84868379116737,-22.5127927449768,11.9157393755432));
#5086=CARTESIAN_POINT('Ctrl Pts',(-3.12606319175256,-23.2393767520925,11.8175853786087));
#5087=CARTESIAN_POINT('Ctrl Pts',(-4.33213271301493,-24.880386526967,11.6703268381421));
#5088=CARTESIAN_POINT('Ctrl Pts',(-4.61678084393395,-25.5145917668544,11.6212300753262));
#5089=CARTESIAN_POINT('Ctrl Pts',(-4.8325074990541,-26.51374965466,11.547605629606));
#5090=CARTESIAN_POINT('Ctrl Pts',(-4.86981537831802,-26.8545716453141,11.5230623381901));
#5091=CARTESIAN_POINT('Ctrl Pts',(-4.87150546249911,-27.5373956033118,11.4739637523339));
#5092=CARTESIAN_POINT('Ctrl Pts',(-4.84806449389349,-27.8775537395237,11.4494246411902));
#5093=CARTESIAN_POINT('Ctrl Pts',(-4.8332020483632,-28.2179636982637,11.4248805192881));
#5094=CARTESIAN_POINT('Ctrl Pts',(-4.49992531496781,-27.2005618150104,22.4987331790167));
#5095=CARTESIAN_POINT('Ctrl Pts',(-4.50123266577206,-27.9399345555106,22.4403537839278));
#5096=CARTESIAN_POINT('Ctrl Pts',(-4.31885456358521,-28.6714666153785,22.3845992765752));
#5097=CARTESIAN_POINT('Ctrl Pts',(-3.27206873853112,-30.6387455869407,22.2092430694354));
#5098=CARTESIAN_POINT('Ctrl Pts',(-1.90301347052226,-31.5589454854703,22.0978648836455));
#5099=CARTESIAN_POINT('Ctrl Pts',(1.08133745456905,-31.8588483286696,21.8641055935273));
#5100=CARTESIAN_POINT('Ctrl Pts',(2.62163729847883,-31.2259625043182,21.7526920522415));
#5101=CARTESIAN_POINT('Ctrl Pts',(4.54712383673962,-28.889667640373,21.5189807362004));
#5102=CARTESIAN_POINT('Ctrl Pts',(4.87991725612086,-27.2420071964223,21.4075326300492));
#5103=CARTESIAN_POINT('Ctrl Pts',(3.99926793651637,-24.3160463481836,21.1738683059317));
#5104=CARTESIAN_POINT('Ctrl Pts',(2.80324492166405,-23.1127118024641,21.0623863989465));
#5105=CARTESIAN_POINT('Ctrl Pts',(-0.145664295624094,-22.2108911563125,
20.8287681139101));
#5106=CARTESIAN_POINT('Ctrl Pts',(-1.82608753442347,-22.5396643242445,20.7172531447498));
#5107=CARTESIAN_POINT('Ctrl Pts',(-4.23617685498116,-24.5081432429562,20.4836799735107));
#5108=CARTESIAN_POINT('Ctrl Pts',(-4.90258935139331,-26.1024197715759,20.3721326565532));
#5109=CARTESIAN_POINT('Ctrl Pts',(-4.60239401978947,-29.2279523583354,20.1386037010885));
#5110=CARTESIAN_POINT('Ctrl Pts',(-3.63850146388098,-30.6809230335259,20.0270247275001));
#5111=CARTESIAN_POINT('Ctrl Pts',(-0.848312218451317,-32.1812843569572,
19.7935391153079));
#5112=CARTESIAN_POINT('Ctrl Pts',(0.910962191510308,-32.187257662144,19.6819291541039));
#5113=CARTESIAN_POINT('Ctrl Pts',(3.73351916376344,-30.6878849222468,19.4484860378945));
#5114=CARTESIAN_POINT('Ctrl Pts',(4.72474370347859,-29.2155039993741,19.3368457367663));
#5115=CARTESIAN_POINT('Ctrl Pts',(5.04923349895883,-26.0077171480983,19.103444293163));
#5116=CARTESIAN_POINT('Ctrl Pts',(4.36986673206198,-24.3509968931086,18.9917742794446));
#5117=CARTESIAN_POINT('Ctrl Pts',(1.86145168328288,-22.2810150440159,18.7584137083719));
#5118=CARTESIAN_POINT('Ctrl Pts',(0.0911844603756664,-21.9222328729832,
18.6467145899854));
#5119=CARTESIAN_POINT('Ctrl Pts',(-3.05047794174479,-22.8657614168808,18.4133941133931));
#5120=CARTESIAN_POINT('Ctrl Pts',(-4.3434939460169,-24.1492993667947,18.3016664794364));
#5121=CARTESIAN_POINT('Ctrl Pts',(-5.31279863706187,-27.3124610697944,18.0683853413922));
#5122=CARTESIAN_POINT('Ctrl Pts',(-4.96105242549078,-29.116041915327,17.9566297629436));
#5123=CARTESIAN_POINT('Ctrl Pts',(-2.85190795720616,-31.7012004702625,17.7233872278977));
#5124=CARTESIAN_POINT('Ctrl Pts',(-1.14247440761136,-32.4168925823255,17.6116042590234));
#5125=CARTESIAN_POINT('Ctrl Pts',(1.36942113919458,-32.1769364386145,17.4367007733733));
#5126=CARTESIAN_POINT('Ctrl Pts',(2.17863030294074,-31.8896680393015,17.3807991645495));
#5127=CARTESIAN_POINT('Ctrl Pts',(3.58594774059714,-30.955345510934,17.2642061815091));
#5128=CARTESIAN_POINT('Ctrl Pts',(4.1666380278044,-30.3178934995088,17.2082979257248));
#5129=CARTESIAN_POINT('Ctrl Pts',(4.97070480320723,-28.8243377732163,17.0917141975888));
#5130=CARTESIAN_POINT('Ctrl Pts',(5.18324736692089,-27.9849325707496,17.0357993595099));
#5131=CARTESIAN_POINT('Ctrl Pts',(5.18837634682399,-26.2816906794162,16.9192248016874));
#5132=CARTESIAN_POINT('Ctrl Pts',(4.97928961288882,-25.4377044137181,16.8633034450976));
#5133=CARTESIAN_POINT('Ctrl Pts',(4.17766130573194,-23.9269514586941,16.7467379739209));
#5134=CARTESIAN_POINT('Ctrl Pts',(3.59301796923098,-23.2784899136664,16.6908101616495));
#5135=CARTESIAN_POINT('Ctrl Pts',(2.16808835767185,-22.3200655571735,16.5742536948244));
#5136=CARTESIAN_POINT('Ctrl Pts',(1.34341569002319,-22.0225242875423,16.5183194887516));
#5137=CARTESIAN_POINT('Ctrl Pts',(-0.37202542262785,-21.848229520912,16.4017719448942));
#5138=CARTESIAN_POINT('Ctrl Pts',(-1.2431512747268,-21.9750627042462,16.3458314060321));
#5139=CARTESIAN_POINT('Ctrl Pts',(-2.84469319036191,-22.6326276198057,16.2292927049662));
#5140=CARTESIAN_POINT('Ctrl Pts',(-3.55608395141779,-23.1572481132965,16.1733458934499));
#5141=CARTESIAN_POINT('Ctrl Pts',(-4.66303405570225,-24.4975081087771,16.0568159559262));
#5142=CARTESIAN_POINT('Ctrl Pts',(-5.0446924336988,-25.2987711172549,16.0008629310603));
#5143=CARTESIAN_POINT('Ctrl Pts',(-5.39056519898843,-27.0094466251327,15.8843416789414));
#5144=CARTESIAN_POINT('Ctrl Pts',(-5.34930304043553,-27.8996098051487,15.8283824991195));
#5145=CARTESIAN_POINT('Ctrl Pts',(-4.84595092330871,-29.5780539034839,15.7118698553524));
#5146=CARTESIAN_POINT('Ctrl Pts',(-4.38811855967175,-30.3467642405488,15.6559045781531));
#5147=CARTESIAN_POINT('Ctrl Pts',(-3.14807661476919,-31.5947342749175,15.5394004666024));
#5148=CARTESIAN_POINT('Ctrl Pts',(-2.37886502949379,-32.0587365058605,15.4834291488454));
#5149=CARTESIAN_POINT('Ctrl Pts',(-0.690271412805203,-32.5768833169426,
15.3669334943444));
#5150=CARTESIAN_POINT('Ctrl Pts',(0.210437406783647,-32.6237032613599,15.3109561919855));
#5151=CARTESIAN_POINT('Ctrl Pts',(1.95077582228988,-32.2833593081943,15.1944689204932));
#5152=CARTESIAN_POINT('Ctrl Pts',(2.77047067840731,-31.8985499371097,15.1384856887274));
#5153=CARTESIAN_POINT('Ctrl Pts',(4.15032302098314,-30.7736043375475,15.0220067269618));
#5154=CARTESIAN_POINT('Ctrl Pts',(4.69400309684405,-30.0449584837519,14.9660176202321));
#5155=CARTESIAN_POINT('Ctrl Pts',(5.38335863834062,-28.395939593178,14.8495468960155));
#5156=CARTESIAN_POINT('Ctrl Pts',(5.51992097583071,-27.4934852178884,14.7935519679768));
#5157=CARTESIAN_POINT('Ctrl Pts',(5.34990401728289,-25.7072478702335,14.6770894099612));
#5158=CARTESIAN_POINT('Ctrl Pts',(5.04374456081733,-24.8435781449226,14.6210887135337));
#5159=CARTESIAN_POINT('Ctrl Pts',(4.0479320191368,-23.342552408645,14.5046342513644));
#5160=CARTESIAN_POINT('Ctrl Pts',(3.36814614645295,-22.7227447945842,14.4486278387742));
#5161=CARTESIAN_POINT('Ctrl Pts',(1.77619102970885,-21.8650344590564,14.3321814028423));
#5162=CARTESIAN_POINT('Ctrl Pts',(0.881013595157293,-21.6379564042767,14.2761693255965));
#5163=CARTESIAN_POINT('Ctrl Pts',(-0.934286602741275,-21.631913240891,14.1597308473328));
#5164=CARTESIAN_POINT('Ctrl Pts',(-1.83430603011931,-21.85447637771,14.1037131561842));
#5165=CARTESIAN_POINT('Ctrl Pts',(-3.44430347736566,-22.7081266226923,13.9872825678333));
#5166=CARTESIAN_POINT('Ctrl Pts',(-4.13582211102842,-23.3310704412515,13.9312593128857));
#5167=CARTESIAN_POINT('Ctrl Pts',(-5.15723598600513,-24.8486604334571,13.8148365475172));
#5168=CARTESIAN_POINT('Ctrl Pts',(-5.47468869489397,-25.7274061109226,13.7588077782201));
#5169=CARTESIAN_POINT('Ctrl Pts',(-5.66084498304722,-27.5542511137055,13.6423927697258));
#5170=CARTESIAN_POINT('Ctrl Pts',(-5.52607729259019,-28.4824463986154,13.5863585348362));
#5171=CARTESIAN_POINT('Ctrl Pts',(-4.82645265952584,-30.1878171234494,13.4699512180057));
#5172=CARTESIAN_POINT('Ctrl Pts',(-4.26793016275464,-30.9457917464557,13.4139115656321));
#5173=CARTESIAN_POINT('Ctrl Pts',(-2.84163338331343,-32.1244708835282,13.2975118759857));
#5174=CARTESIAN_POINT('Ctrl Pts',(-1.98851329456531,-32.5312245863753,13.2414668535995));
#5175=CARTESIAN_POINT('Ctrl Pts',(-0.168154346495923,-32.8997884885716,
13.1250747275302));
#5176=CARTESIAN_POINT('Ctrl Pts',(0.779568298212397,-32.8562079727566,13.0690243819638));
#5177=CARTESIAN_POINT('Ctrl Pts',(2.56542990953642,-32.3211571768756,12.9526397565944));
#5178=CARTESIAN_POINT('Ctrl Pts',(3.38380416962575,-31.8341443288812,12.8965841340846));
#5179=CARTESIAN_POINT('Ctrl Pts',(4.71155278837089,-30.5155103343138,12.7802069473221));
#5180=CARTESIAN_POINT('Ctrl Pts',(5.20559259369133,-29.6971531119313,12.7241460934996));
#5181=CARTESIAN_POINT('Ctrl Pts',(5.75703886090729,-27.9016459598323,12.6077762839981));
#5182=CARTESIAN_POINT('Ctrl Pts',(5.80717713818053,-26.9434385648419,12.5517102438793));
#5183=CARTESIAN_POINT('Ctrl Pts',(5.44579520263474,-25.0931237590171,12.4353477510898));
#5184=CARTESIAN_POINT('Ctrl Pts',(5.0368047411671,-24.2211610859936,12.3792765691091));
#5185=CARTESIAN_POINT('Ctrl Pts',(3.84146164273372,-22.7542474974693,12.2629213331626));
#5186=CARTESIAN_POINT('Ctrl Pts',(3.06685116348872,-22.1758765063834,12.2068450531984));
#5187=CARTESIAN_POINT('Ctrl Pts',(1.3147114679644,-21.4429359570459,12.0904970149672));
#5188=CARTESIAN_POINT('Ctrl Pts',(0.355369734306315,-21.2974519808943,12.0344156803179));
#5189=CARTESIAN_POINT('Ctrl Pts',(-2.21947927012219,-21.541945111076,11.8765628382364));
#5190=CARTESIAN_POINT('Ctrl Pts',(-3.75768230547338,-22.4163266113853,11.7792514363029));
#5191=CARTESIAN_POINT('Ctrl Pts',(-5.21498730250992,-24.3919766537203,11.6318625545005));
#5192=CARTESIAN_POINT('Ctrl Pts',(-5.56061254440886,-25.1583366949337,11.5821196744937));
#5193=CARTESIAN_POINT('Ctrl Pts',(-5.82237026188237,-26.3605430038448,11.5086720015383));
#5194=CARTESIAN_POINT('Ctrl Pts',(-5.86810470583882,-26.7709263784967,11.4841148639085));
#5195=CARTESIAN_POINT('Ctrl Pts',(-5.87151787372438,-27.5964966533761,11.4342490225503));
#5196=CARTESIAN_POINT('Ctrl Pts',(-5.8464491178956,-27.9182877595946,11.4098155239949));
#5197=CARTESIAN_POINT('Ctrl Pts',(-5.83158667236532,-28.2586977183358,11.3852714020937));
#5198=CARTESIAN_POINT('Ctrl Pts',(-4.49992531496781,-27.1010184425723,21.5036999549465));
#5199=CARTESIAN_POINT('Ctrl Pts',(-4.51674600628465,-27.8405511731054,21.4453045543583));
#5200=CARTESIAN_POINT('Ctrl Pts',(-4.3513754570227,-28.5765453512511,21.3895276624965));
#5201=CARTESIAN_POINT('Ctrl Pts',(-3.34502119885618,-30.5657740901924,21.2141080231263));
#5202=CARTESIAN_POINT('Ctrl Pts',(-1.99683196222126,-31.5170666924607,21.1026952188504));
#5203=CARTESIAN_POINT('Ctrl Pts',(0.980993279522333,-31.8772272555485,20.8688610765165));
#5204=CARTESIAN_POINT('Ctrl Pts',(2.53490239289457,-31.2787547245274,20.7574094693259));
#5205=CARTESIAN_POINT('Ctrl Pts',(4.50569444399399,-28.9816631968142,20.5236326621716));
#5206=CARTESIAN_POINT('Ctrl Pts',(4.87413701918684,-27.3422265898772,20.41214314674));
#5207=CARTESIAN_POINT('Ctrl Pts',(4.05086560996824,-24.4015014064168,20.1784223463925));
#5208=CARTESIAN_POINT('Ctrl Pts',(2.88154677707693,-23.173754043832,20.0668957873436));
#5209=CARTESIAN_POINT('Ctrl Pts',(-0.0470467715653138,-22.2169532717186,
19.8332297105388));
#5210=CARTESIAN_POINT('Ctrl Pts',(-1.73235777827075,-22.5102673549153,19.7216669438178));
#5211=CARTESIAN_POINT('Ctrl Pts',(-4.17572182242301,-24.4312269013205,19.4880543497385));
#5212=CARTESIAN_POINT('Ctrl Pts',(-4.87376845888169,-26.0095620732211,19.3764561838128));
#5213=CARTESIAN_POINT('Ctrl Pts',(-4.6310120681261,-29.1353686231182,19.1428958730047));
#5214=CARTESIAN_POINT('Ctrl Pts',(-3.69789395427398,-30.6051559498652,19.0312630900414));
#5215=CARTESIAN_POINT('Ctrl Pts',(-0.939901316815822,-32.1524297385279,
18.797753901872));
#5216=CARTESIAN_POINT('Ctrl Pts',(0.815770716897848,-32.192946710534,18.6860872589115));
#5217=CARTESIAN_POINT('Ctrl Pts',(3.65834639903831,-30.746287086809,18.4526280705631));
#5218=CARTESIAN_POINT('Ctrl Pts',(4.67570856491877,-29.2962834910467,18.3409283004432));
#5219=CARTESIAN_POINT('Ctrl Pts',(5.05445235298275,-26.1019770515496,18.1075180249339));
#5220=CARTESIAN_POINT('Ctrl Pts',(4.40805306181254,-24.4365392522985,17.9957858373769));
#5221=CARTESIAN_POINT('Ctrl Pts',(1.94130016670179,-22.3299662886282,17.7624234222861));
#5222=CARTESIAN_POINT('Ctrl Pts',(0.182492857305352,-21.939377617945,17.6506595049407));
#5223=CARTESIAN_POINT('Ctrl Pts',(-2.96543044577777,-22.8282401952741,17.4173439305767));
#5224=CARTESIAN_POINT('Ctrl Pts',(-4.27794385851622,-24.0844995025642,17.3055489496951));
#5225=CARTESIAN_POINT('Ctrl Pts',(-5.29537653242634,-27.2218242153782,17.0722792286103));
#5226=CARTESIAN_POINT('Ctrl Pts',(-4.97689278167529,-29.0259395054587,16.9604538299531));
#5227=CARTESIAN_POINT('Ctrl Pts',(-2.91608530249191,-31.6357336752382,16.7272290046934));
#5228=CARTESIAN_POINT('Ctrl Pts',(-1.22497985084763,-32.3788890909175,16.6153738146158));
#5229=CARTESIAN_POINT('Ctrl Pts',(1.28145612063066,-32.1789932923933,16.4404881713498));
#5230=CARTESIAN_POINT('Ctrl Pts',(2.0927818601203,-31.9069109397873,16.3845495671917));
#5231=CARTESIAN_POINT('Ctrl Pts',(3.50922640420288,-30.9978632225545,16.2679699605668));
#5232=CARTESIAN_POINT('Ctrl Pts',(4.09881550944335,-30.3728309488599,16.2120241353908));
#5233=CARTESIAN_POINT('Ctrl Pts',(4.92262783581331,-28.8973868790768,16.0954552401651));
#5234=CARTESIAN_POINT('Ctrl Pts',(5.14877399302525,-28.064821040575,16.0395022670422));
#5235=CARTESIAN_POINT('Ctrl Pts',(5.17972192673461,-26.3684552205223,15.9229439741396));
#5236=CARTESIAN_POINT('Ctrl Pts',(4.98580796318786,-25.5242055246215,15.8669839251149));
#5237=CARTESIAN_POINT('Ctrl Pts',(4.21017429044416,-24.0075929294983,15.7504361268929));
#5238=CARTESIAN_POINT('Ctrl Pts',(3.63880072013838,-23.351872300329,15.6944690729279));
#5239=CARTESIAN_POINT('Ctrl Pts',(2.23413550967172,-22.3762507712042,15.5779316635816));
#5240=CARTESIAN_POINT('Ctrl Pts',(1.41781408360257,-22.0661561590653,15.5219576745624));
#5241=CARTESIAN_POINT('Ctrl Pts',(-0.2876678119969,-21.8672909533799,15.4054305496812));
#5242=CARTESIAN_POINT('Ctrl Pts',(-1.15723576718454,-21.9791742088117,15.349449694498));
#5243=CARTESIAN_POINT('Ctrl Pts',(-2.76133682475571,-22.6104139372597,15.2329327513282));
#5244=CARTESIAN_POINT('Ctrl Pts',(-3.47827719059933,-23.1211141138698,15.1769450978676));
#5245=CARTESIAN_POINT('Ctrl Pts',(-4.59966549973914,-24.4392847330131,15.0604382350449));
#5246=CARTESIAN_POINT('Ctrl Pts',(-4.99267244674646,-25.2308278340738,15.0044438502435));
#5247=CARTESIAN_POINT('Ctrl Pts',(-5.36152867501004,-26.9286517721488,14.8879469679338));
#5248=CARTESIAN_POINT('Ctrl Pts',(-5.33479062947237,-27.815489816777,14.8319459176988));
#5249=CARTESIAN_POINT('Ctrl Pts',(-4.85770689425811,-29.4932029850683,14.7154589175941));
#5250=CARTESIAN_POINT('Ctrl Pts',(-4.41424130928336,-30.2657064039853,14.6594512668976));
#5251=CARTESIAN_POINT('Ctrl Pts',(-3.19776731478627,-31.5251842790945,14.5429740520141));
#5252=CARTESIAN_POINT('Ctrl Pts',(-2.43948640778453,-31.9991936236663,14.4869598649523));
#5253=CARTESIAN_POINT('Ctrl Pts',(-0.76641117646687,-32.538424291025,14.3704923396933));
#5254=CARTESIAN_POINT('Ctrl Pts',(0.129280639488567,-32.5991484080323,14.3144716793848));
#5255=CARTESIAN_POINT('Ctrl Pts',(1.86565117755554,-32.2846351962422,14.1980137496642));
#5256=CARTESIAN_POINT('Ctrl Pts',(2.6873584363981,-31.9144328140864,14.1419866783607));
#5257=CARTESIAN_POINT('Ctrl Pts',(4.0756575425974,-30.8141731242952,14.025538251239));
#5258=CARTESIAN_POINT('Ctrl Pts',(4.62788574697171,-30.0974982118229,13.9695048303297));
#5259=CARTESIAN_POINT('Ctrl Pts',(5.33614212196108,-28.4664074366612,13.8530658143517));
#5260=CARTESIAN_POINT('Ctrl Pts',(5.48580553915912,-27.5705664905401,13.7970261043234));
#5261=CARTESIAN_POINT('Ctrl Pts',(5.34081184824442,-25.791439376031,13.6805964092432));
#5262=CARTESIAN_POINT('Ctrl Pts',(5.04929361698828,-24.927539264489,13.6245504697451));
#5263=CARTESIAN_POINT('Ctrl Pts',(4.07891464172889,-23.4212168574546,13.5081300066553));
#5264=CARTESIAN_POINT('Ctrl Pts',(3.41195903484832,-22.794417393971,13.4520778965404));
#5265=CARTESIAN_POINT('Ctrl Pts',(1.84005664325852,-21.9202404356125,13.3356665776424));
#5266=CARTESIAN_POINT('Ctrl Pts',(0.952974962988242,-21.6810345955686,13.2796083549412));
#5267=CARTESIAN_POINT('Ctrl Pts',(-0.852207019879878,-21.6511301665541,
13.1632060938123));
#5268=CARTESIAN_POINT('Ctrl Pts',(-1.75069597922114,-21.8592211322789,13.1071418157038));
#5269=CARTESIAN_POINT('Ctrl Pts',(-3.36279321619093,-22.687065563139,12.9907485270725));
#5270=CARTESIAN_POINT('Ctrl Pts',(-4.0596712085529,-23.2965088909024,12.9346782499817));
#5271=CARTESIAN_POINT('Ctrl Pts',(-5.09490115062812,-24.7922309126811,12.8182938497412));
#5272=CARTESIAN_POINT('Ctrl Pts',(-5.42335290963779,-25.6615296657728,12.7622176293468));
#5273=CARTESIAN_POINT('Ctrl Pts',(-5.6318733184926,-27.4754205110425,12.6458420345123));
#5274=CARTESIAN_POINT('Ctrl Pts',(-5.51121048465282,-28.4003675711241,12.5897599257099));
#5275=CARTESIAN_POINT('Ctrl Pts',(-4.83738798718038,-30.1046366902265,12.4733930545196));
#5276=CARTESIAN_POINT('Ctrl Pts',(-4.29284127804266,-30.8662836546237,12.4173051114547));
#5277=CARTESIAN_POINT('Ctrl Pts',(-2.88989812922953,-32.0559489908963,12.3009468831881));
#5278=CARTESIAN_POINT('Ctrl Pts',(-2.04742969825749,-32.4724339533943,12.244853159285));
#5279=CARTESIAN_POINT('Ctrl Pts',(-0.2426536662203,-32.8615528897918,12.1285034943741));
#5280=CARTESIAN_POINT('Ctrl Pts',(0.700167228706349,-32.8315189484388,12.0724040423241));
#5281=CARTESIAN_POINT('Ctrl Pts',(2.48176316317964,-32.3218947112272,11.9560628622509));
#5282=CARTESIAN_POINT('Ctrl Pts',(3.30209026051788,-31.8491345603716,11.8999577340539));
#5283=CARTESIAN_POINT('Ctrl Pts',(4.63785467742761,-30.5549942620067,11.7836249613568));
#5284=CARTESIAN_POINT('Ctrl Pts',(5.14023670521377,-29.7483336343732,11.7275142083257));
#5285=CARTESIAN_POINT('Ctrl Pts',(5.71014369190083,-27.9707987230122,11.6111897665715));
#5286=CARTESIAN_POINT('Ctrl Pts',(5.77308874181379,-27.0190622633568,11.5550734393245));
#5287=CARTESIAN_POINT('Ctrl Pts',(5.43639437006847,-25.1760989492496,11.4387572531387));
#5288=CARTESIAN_POINT('Ctrl Pts',(5.04173404968112,-24.3039132848956,11.3826354016244));
#5289=CARTESIAN_POINT('Ctrl Pts',(3.87166745943498,-22.8320547671859,11.2663273965984));
#5290=CARTESIAN_POINT('Ctrl Pts',(3.10962740498996,-22.2468328201306,11.2102000701237));
#5291=CARTESIAN_POINT('Ctrl Pts',(1.3775808247441,-21.4977812085784,11.0939001728392));
#5292=CARTESIAN_POINT('Ctrl Pts',(0.426176004646674,-21.3404003073863,11.0377674200549));
#5293=CARTESIAN_POINT('Ctrl Pts',(-2.13467139062884,-21.5528754416251,10.8799811119317));
#5294=CARTESIAN_POINT('Ctrl Pts',(-3.67375330512296,-22.4019087871921,10.7826247286485));
#5295=CARTESIAN_POINT('Ctrl Pts',(-5.14572845587871,-24.3467779409998,10.6352234649416));
#5296=CARTESIAN_POINT('Ctrl Pts',(-5.4980087978572,-25.10396329861,10.585497622957));
#5297=CARTESIAN_POINT('Ctrl Pts',(-5.77284291612865,-26.2950238657267,10.5120341100286));
#5298=CARTESIAN_POINT('Ctrl Pts',(-5.82326382778836,-26.7021580375338,10.4874753114238));
#5299=CARTESIAN_POINT('Ctrl Pts',(-5.83613711196663,-27.5221379313639,10.4376301541696));
#5300=CARTESIAN_POINT('Ctrl Pts',(-5.80990657648216,-27.8448337026384,10.4131866340964));
#5301=CARTESIAN_POINT('Ctrl Pts',(-5.79504413095202,-28.1852436613808,10.3886425121934));
#5302=CARTESIAN_POINT('Ctrl Pts',(-3.5,-27.1131792176833,21.5024833879649));
#5303=CARTESIAN_POINT('Ctrl Pts',(-3.51479119919922,-27.6859453885664,21.4451837185487));
#5304=CARTESIAN_POINT('Ctrl Pts',(-3.3869826954375,-28.2639018202575,21.3878808596267));
#5305=CARTESIAN_POINT('Ctrl Pts',(-2.61104013965461,-29.8091522948055,21.2159741435134));
#5306=CARTESIAN_POINT('Ctrl Pts',(-1.55527081107218,-30.5598658867912,21.1013735009366));
#5307=CARTESIAN_POINT('Ctrl Pts',(0.7596584103706,-30.8465909355752,20.8721694081605));
#5308=CARTESIAN_POINT('Ctrl Pts',(1.98433800521209,-30.3798149635844,20.7575670418755));
#5309=CARTESIAN_POINT('Ctrl Pts',(3.52578602540974,-28.5931135200025,20.5283676296524));
#5310=CARTESIAN_POINT('Ctrl Pts',(3.8208190800791,-27.3005795704328,20.4137635916772));
#5311=CARTESIAN_POINT('Ctrl Pts',(3.18340034511317,-25.0004020130352,20.1845686868986));
#5312=CARTESIAN_POINT('Ctrl Pts',(2.26172892311522,-24.0264166801336,20.0699630275308));
#5313=CARTESIAN_POINT('Ctrl Pts',(-0.0310075805132356,-23.2709470686081,
19.840772464982));
#5314=CARTESIAN_POINT('Ctrl Pts',(-1.36774615552683,-23.4993356660845,19.7261652328664));
#5315=CARTESIAN_POINT('Ctrl Pts',(-3.29044999554861,-25.003443698954,19.4969788547815));
#5316=CARTESIAN_POINT('Ctrl Pts',(-3.84882652597964,-26.255889878113,19.3823700969656));
#5317=CARTESIAN_POINT('Ctrl Pts',(-3.66341653596594,-28.7171925636406,19.1531877526223));
#5318=CARTESIAN_POINT('Ctrl Pts',(-2.92366288113256,-29.8898022514147,19.0385775146034));
#5319=CARTESIAN_POINT('Ctrl Pts',(-0.750050065449063,-31.1155888685023,
18.8093990599493));
#5320=CARTESIAN_POINT('Ctrl Pts',(0.651110587682156,-31.1517796318851,18.6947873857344));
#5321=CARTESIAN_POINT('Ctrl Pts',(2.90172211077653,-30.0124147872479,18.4656126830036));
#5322=CARTESIAN_POINT('Ctrl Pts',(3.71853772096227,-28.8547645355866,18.3509996151738));
#5323=CARTESIAN_POINT('Ctrl Pts',(4.02392234264642,-26.3233804905586,18.1218285325501));
#5324=CARTESIAN_POINT('Ctrl Pts',(3.50918503257104,-24.9871031169595,18.0072141122992));
#5325=CARTESIAN_POINT('Ctrl Pts',(1.55288051607053,-23.3098136929698,17.7780465236243));
#5326=CARTESIAN_POINT('Ctrl Pts',(0.140896517323791,-22.9926200323223,17.6634307908027));
#5327=CARTESIAN_POINT('Ctrl Pts',(-2.36650964254058,-23.6955465860942,17.4342665752667));
#5328=CARTESIAN_POINT('Ctrl Pts',(-3.42532249325332,-24.7042160076948,17.319649568463));
#5329=CARTESIAN_POINT('Ctrl Pts',(-4.24151789226149,-27.205672166438,17.0904886102752));
#5330=CARTESIAN_POINT('Ctrl Pts',(-3.98794903777075,-28.6613021650618,16.9758703668355));
#5331=CARTESIAN_POINT('Ctrl Pts',(-2.34405122024042,-30.7505189403242,16.7467125550671));
#5332=CARTESIAN_POINT('Ctrl Pts',(-0.978754765971974,-31.3540484715026,
16.6320931111307));
#5333=CARTESIAN_POINT('Ctrl Pts',(1.02933886603348,-31.1972354808515,16.460227032321));
#5334=CARTESIAN_POINT('Ctrl Pts',(1.68709482472537,-30.9779968406706,16.4029168679907));
#5335=CARTESIAN_POINT('Ctrl Pts',(2.8240837151474,-30.2508925065775,16.2883402228593));
#5336=CARTESIAN_POINT('Ctrl Pts',(3.30314935266293,-29.7448544918448,16.2310297714992));
#5337=CARTESIAN_POINT('Ctrl Pts',(3.96627580118359,-28.5616040731508,16.116453854622));
#5338=CARTESIAN_POINT('Ctrl Pts',(4.15104388235541,-27.8860791480164,16.0591431204344));
#5339=CARTESIAN_POINT('Ctrl Pts',(4.17802239058402,-26.5231491652539,15.9445679195579));
#5340=CARTESIAN_POINT('Ctrl Pts',(4.02164463287101,-25.836899273559,15.8872569066736));
#5341=CARTESIAN_POINT('Ctrl Pts',(3.39969277305442,-24.6162176795914,15.7726824098211));
#5342=CARTESIAN_POINT('Ctrl Pts',(2.9359020278153,-24.0821430128742,15.7153711223063));
#5343=CARTESIAN_POINT('Ctrl Pts',(1.80627259289743,-23.295059368917,15.6007973177115));
#5344=CARTESIAN_POINT('Ctrl Pts',(1.14217129355625,-23.0415308728188,15.5434857595736));
#5345=CARTESIAN_POINT('Ctrl Pts',(-0.231877317222814,-22.8792861228552,
15.4289126357253));
#5346=CARTESIAN_POINT('Ctrl Pts',(-0.940537550161687,-22.9692999005262,
15.3716008109));
#5347=CARTESIAN_POINT('Ctrl Pts',(-2.23508230276584,-23.4765970744679,15.2570283565139));
#5348=CARTESIAN_POINT('Ctrl Pts',(-2.82042721228882,-23.8921601369938,15.1997162688729));
#5349=CARTESIAN_POINT('Ctrl Pts',(-3.72724254909164,-24.9550994865649,15.0851444728953));
#5350=CARTESIAN_POINT('Ctrl Pts',(-4.04904226418634,-25.6007082903028,15.0278321262568));
#5351=CARTESIAN_POINT('Ctrl Pts',(-4.34898179372202,-26.9722920315092,14.913260977831));
#5352=CARTESIAN_POINT('Ctrl Pts',(-4.32823823833014,-27.696864249156,14.8559483759565));
#5353=CARTESIAN_POINT('Ctrl Pts',(-3.94416673686108,-29.0543767984046,14.741377864454));
#5354=CARTESIAN_POINT('Ctrl Pts',(-3.58247834736109,-29.6866038630478,14.684065011041));
#5355=CARTESIAN_POINT('Ctrl Pts',(-2.59897553580158,-30.7075411869121,14.5694951260371));
#5356=CARTESIAN_POINT('Ctrl Pts',(-1.97893887953295,-31.0963900092535,14.5121820247212));
#5357=CARTESIAN_POINT('Ctrl Pts',(-0.62377058727827,-31.5350735702099,14.3976127560067));
#5358=CARTESIAN_POINT('Ctrl Pts',(0.109859887125028,-31.5858618602476,14.3402994103674));
#5359=CARTESIAN_POINT('Ctrl Pts',(1.51846868411767,-31.3325375520331,14.2257307479178));
#5360=CARTESIAN_POINT('Ctrl Pts',(2.19257064211805,-31.0299670824768,14.1684171614822));
#5361=CARTESIAN_POINT('Ctrl Pts',(3.32065975230898,-30.1381775844584,14.0538490954731));
#5362=CARTESIAN_POINT('Ctrl Pts',(3.77459621319051,-29.5507269915758,13.9965352717156));
#5363=CARTESIAN_POINT('Ctrl Pts',(4.35164549000208,-28.2261503388289,13.8819677925012));
#5364=CARTESIAN_POINT('Ctrl Pts',(4.47554085920862,-27.4906059318028,13.8246537348364));
#5365=CARTESIAN_POINT('Ctrl Pts',(4.35932633846837,-26.043646007592,13.7100868329779));
#5366=CARTESIAN_POINT('Ctrl Pts',(4.1206457473642,-25.3332578752253,13.6527725447744));
#5367=CARTESIAN_POINT('Ctrl Pts',(3.33223129728641,-24.106308328171,13.5382062109767));
#5368=CARTESIAN_POINT('Ctrl Pts',(2.78423731477771,-23.5899834651597,13.4808916955503));
#5369=CARTESIAN_POINT('Ctrl Pts',(1.50450674316234,-22.8764080003258,13.3663259207328));
#5370=CARTESIAN_POINT('Ctrl Pts',(0.774413779611081,-22.6785518889991,13.309011181339));
#5371=CARTESIAN_POINT('Ctrl Pts',(-0.69739330426496,-22.6525522223851,13.1944459565731));
#5372=CARTESIAN_POINT('Ctrl Pts',(-1.43794247925327,-22.8231062186778,13.1371309964266));
#5373=CARTESIAN_POINT('Ctrl Pts',(-2.7541948376007,-23.4972409646481,13.0225663129528));
#5374=CARTESIAN_POINT('Ctrl Pts',(-3.32948087019843,-23.9991290609593,12.9652511352145));
#5375=CARTESIAN_POINT('Ctrl Pts',(-4.17626345911414,-25.2198325829076,12.8506869844455));
#5376=CARTESIAN_POINT('Ctrl Pts',(-4.4481843446811,-25.936961310921,12.7933715922294));
#5377=CARTESIAN_POINT('Ctrl Pts',(-4.62015665278908,-27.4194785452993,12.6788079657272));
#5378=CARTESIAN_POINT('Ctrl Pts',(-4.52137115313415,-28.183579240772,12.621492362104));
#5379=CARTESIAN_POINT('Ctrl Pts',(-3.97152663554103,-29.5783806208201,12.5069292515898));
#5380=CARTESIAN_POINT('Ctrl Pts',(-3.5220951227733,-30.2084906103522,12.4496134395774));
#5381=CARTESIAN_POINT('Ctrl Pts',(-2.37437165907619,-31.183679244984,12.3350508369351));
#5382=CARTESIAN_POINT('Ctrl Pts',(-1.67779038310627,-31.5289988293348,12.277734819509));
#5383=CARTESIAN_POINT('Ctrl Pts',(-0.199197333900588,-31.8492812709321,
12.1631727167557));
#5384=CARTESIAN_POINT('Ctrl Pts',(0.581419535730091,-31.825256919753,12.1058564968451));
#5385=CARTESIAN_POINT('Ctrl Pts',(2.04290487097247,-31.4086885823989,11.9912948861633));
#5386=CARTESIAN_POINT('Ctrl Pts',(2.72301785637377,-31.017689933097,11.9339784666505));
#5387=CARTESIAN_POINT('Ctrl Pts',(3.82034316796606,-29.9565159886648,11.8194173403514));
#5388=CARTESIAN_POINT('Ctrl Pts',(4.23761275995296,-29.2880562452814,11.7621007240815));
#5389=CARTESIAN_POINT('Ctrl Pts',(4.70706068115205,-27.8283747226536,11.6475400746183));
#5390=CARTESIAN_POINT('Ctrl Pts',(4.76009229327592,-27.0386382546772,11.5902232643864));
#5391=CARTESIAN_POINT('Ctrl Pts',(4.48463927434238,-25.5233462828554,11.4756630843606));
#5392=CARTESIAN_POINT('Ctrl Pts',(4.15760185288866,-24.7987006850272,11.4183460829245));
#5393=CARTESIAN_POINT('Ctrl Pts',(3.19600835697949,-23.5869462478655,11.3037863650511));
#5394=CARTESIAN_POINT('Ctrl Pts',(2.56315379146772,-23.099962191222,11.2464691751292));
#5395=CARTESIAN_POINT('Ctrl Pts',(1.13757263913847,-22.4820219779078,11.1319099122695));
#5396=CARTESIAN_POINT('Ctrl Pts',(0.346404347142174,-22.3503795041057,11.0745925365344));
#5397=CARTESIAN_POINT('Ctrl Pts',(-1.76387591167285,-22.5237230755283,10.9191576492385));
#5398=CARTESIAN_POINT('Ctrl Pts',(-3.04213419140331,-23.2249589278969,10.8209586709532));
#5399=CARTESIAN_POINT('Ctrl Pts',(-4.26287386638314,-24.8351878142477,10.6736877485838));
#5400=CARTESIAN_POINT('Ctrl Pts',(-4.55417709738229,-25.4602183705301,10.6246080237907));
#5401=CARTESIAN_POINT('Ctrl Pts',(-4.78298015330037,-26.4482305165422,10.5509677380958));
#5402=CARTESIAN_POINT('Ctrl Pts',(-4.82497450026767,-26.7858033043513,10.5264227857054));
#5403=CARTESIAN_POINT('Ctrl Pts',(-4.83612470074125,-27.4630368812996,10.4773448839533));
#5404=CARTESIAN_POINT('Ctrl Pts',(-4.81152195248019,-27.8040996825675,10.4527957512917));
#5405=CARTESIAN_POINT('Ctrl Pts',(-4.7966595069499,-28.1445096413087,10.4282516293878));
#5406=CARTESIAN_POINT('Ctrl Pts',(-2.5001922552825,-27.1253385629422,21.501266964026));
#5407=CARTESIAN_POINT('Ctrl Pts',(-2.51295420098982,-27.5313577824259,21.4450628969469));
#5408=CARTESIAN_POINT('Ctrl Pts',(-2.42270332621939,-27.9512950495876,21.3862342503864));
#5409=CARTESIAN_POINT('Ctrl Pts',(-1.87714538123526,-29.0526194622768,21.2178400444839));
#5410=CARTESIAN_POINT('Ctrl Pts',(-1.11376157825568,-29.6027776278656,21.100051938429));
#5411=CARTESIAN_POINT('Ctrl Pts',(0.538349565558472,-29.8160757968226,20.8754773508141));
#5412=CARTESIAN_POINT('Ctrl Pts',(1.43383835235719,-29.480980899108,20.7577245958979));
#5413=CARTESIAN_POINT('Ctrl Pts',(2.54599282350851,-28.2046095284856,20.5331020404002));
#5414=CARTESIAN_POINT('Ctrl Pts',(2.76762498907472,-27.2589374478045,20.4153838460841));
#5415=CARTESIAN_POINT('Ctrl Pts',(2.31603707598399,-25.5992322015002,20.190714304724));
#5416=CARTESIAN_POINT('Ctrl Pts',(1.64198394673661,-24.878979061188,20.073029907075));
#5417=CARTESIAN_POINT('Ctrl Pts',(-0.0149702753337169,-24.3248169379275,
19.8483143325555));
#5418=CARTESIAN_POINT('Ctrl Pts',(-1.00317740346447,-24.4882876835594,19.7306629930104));
#5419=CARTESIAN_POINT('Ctrl Pts',(-2.4052822580784,-25.5755932158904,19.5059023104899));
#5420=CARTESIAN_POINT('Ctrl Pts',(-2.82400510475762,-26.5021887200201,19.3882833147663));
#5421=CARTESIAN_POINT('Ctrl Pts',(-2.69593477275153,-28.2990656728991,19.1634784221306));
#5422=CARTESIAN_POINT('Ctrl Pts',(-2.14952284133105,-29.1745326635594,19.0458910791425));
#5423=CARTESIAN_POINT('Ctrl Pts',(-0.560221136608609,-30.0788699092222,
18.8210428488002));
#5424=CARTESIAN_POINT('Ctrl Pts',(0.486469819045022,-30.1107349726532,18.7034864896048));
#5425=CARTESIAN_POINT('Ctrl Pts',(2.14518678566594,-29.2786287756811,18.4785957687259));
#5426=CARTESIAN_POINT('Ctrl Pts',(2.76147942022677,-28.4132974934977,18.361069745729));
#5427=CARTESIAN_POINT('Ctrl Pts',(2.99351350103085,-26.5447578971656,18.1361373575506));
#5428=CARTESIAN_POINT('Ctrl Pts',(2.61042269136205,-25.5376022468545,18.0186410434961));
#5429=CARTESIAN_POINT('Ctrl Pts',(1.1645065354457,-24.2895458878023,17.7936677880135));
#5430=CARTESIAN_POINT('Ctrl Pts',(0.0993050681995977,-24.0457386074764,
17.6762005750292));
#5431=CARTESIAN_POINT('Ctrl Pts',(-1.76765925983151,-24.5627509998687,17.4511872302086));
#5432=CARTESIAN_POINT('Ctrl Pts',(-2.57280137838496,-25.3238596471586,17.3337485292939));
#5433=CARTESIAN_POINT('Ctrl Pts',(-3.18778316377509,-27.1895220166399,17.1086958508986));
#5434=CARTESIAN_POINT('Ctrl Pts',(-2.99912157291404,-28.2967076983704,16.9912850910565));
#5435=CARTESIAN_POINT('Ctrl Pts',(-1.77208439720242,-29.8654082881016,16.7661938145838));
#5436=CARTESIAN_POINT('Ctrl Pts',(-0.732558632003384,-30.3293283518554,
16.6488104418068));
#5437=CARTESIAN_POINT('Ctrl Pts',(0.777251255138965,-30.2155931034426,16.4799635724161));
#5438=CARTESIAN_POINT('Ctrl Pts',(1.28145548961924,-30.0491919623743,16.4212820091803));
#5439=CARTESIAN_POINT('Ctrl Pts',(2.13902158450589,-29.5040096186941,16.308708090036));
#5440=CARTESIAN_POINT('Ctrl Pts',(2.5075767495388,-29.1169518716936,16.2500331729432));
#5441=CARTESIAN_POINT('Ctrl Pts',(3.01003621350007,-28.225860748242,16.1374500000821));
#5442=CARTESIAN_POINT('Ctrl Pts',(3.15343108382589,-27.7073582717565,16.078781664474));
#5443=CARTESIAN_POINT('Ctrl Pts',(3.17644063329496,-26.6778249212213,15.9661893224535));
#5444=CARTESIAN_POINT('Ctrl Pts',(3.05759466794496,-26.1495562562684,15.9075275045547));
#5445=CARTESIAN_POINT('Ctrl Pts',(2.58930655129671,-25.2247708681756,15.7949260770529));
#5446=CARTESIAN_POINT('Ctrl Pts',(2.23308598163984,-24.8123278608962,15.7362707140421));
#5447=CARTESIAN_POINT('Ctrl Pts',(1.37845998383059,-24.2137599340046,15.6236602833198));
#5448=CARTESIAN_POINT('Ctrl Pts',(0.866560913322279,-24.0167909029579,15.5650113133335));
#5449=CARTESIAN_POINT('Ctrl Pts',(-0.176093382241082,-23.8911623029184,
15.4523919607684));
#5450=CARTESIAN_POINT('Ctrl Pts',(-0.723864812305373,-23.9593091742205,
15.3937493227952));
#5451=CARTESIAN_POINT('Ctrl Pts',(-1.7088896572731,-24.3426783667014,15.2811211285617));
#5452=CARTESIAN_POINT('Ctrl Pts',(-2.16265458334177,-24.6631155012729,15.222484762466));
#5453=CARTESIAN_POINT('Ctrl Pts',(-2.85492217708992,-25.4708535911175,15.1098478058101));
#5454=CARTESIAN_POINT('Ctrl Pts',(-3.10552303274938,-25.9705452563459,15.0512176522992));
#5455=CARTESIAN_POINT('Ctrl Pts',(-3.33655396671587,-27.0159271596902,14.9385720113314));
#5456=CARTESIAN_POINT('Ctrl Pts',(-3.32180419664342,-27.5782526294144,14.8799480120284));
#5457=CARTESIAN_POINT('Ctrl Pts',(-3.03073399263118,-28.615602208499,14.7672937637892));
#5458=CARTESIAN_POINT('Ctrl Pts',(-2.7508131833225,-29.1075694124263,14.7086758611242));
#5459=CARTESIAN_POINT('Ctrl Pts',(-2.00025416217446,-29.8899942324127,14.5960130817379));
#5460=CARTESIAN_POINT('Ctrl Pts',(-1.51844550201379,-30.1936925456155,14.5374012188929));
#5461=CARTESIAN_POINT('Ctrl Pts',(-0.481146769632026,-30.5318408224011,
14.4247299835279));
#5462=CARTESIAN_POINT('Ctrl Pts',(0.0904414182347455,-30.572694453714,14.3661241045503));
#5463=CARTESIAN_POINT('Ctrl Pts',(1.1713270120612,-30.3805518545432,14.2534444872335));
#5464=CARTESIAN_POINT('Ctrl Pts',(1.69784102450774,-30.1456053454915,14.194844536933));
#5465=CARTESIAN_POINT('Ctrl Pts',(2.56575073392967,-29.4622615275225,14.0821566109456));
#5466=CARTESIAN_POINT('Ctrl Pts',(2.92140700836645,-29.0040200601594,14.0235625348885));
#5467=CARTESIAN_POINT('Ctrl Pts',(3.36726461420379,-27.9859214901936,13.9108663723842));
#5468=CARTESIAN_POINT('Ctrl Pts',(3.46539496520096,-27.4106547747507,13.8522781169193));
#5469=CARTESIAN_POINT('Ctrl Pts',(3.37795623080819,-26.2958229849414,13.7395737892572));
#5470=CARTESIAN_POINT('Ctrl Pts',(3.19210706725742,-25.7389287819603,13.6809913014795));
#5471=CARTESIAN_POINT('Ctrl Pts',(2.58563574714856,-24.7913192464956,13.5682788789672));
#5472=CARTESIAN_POINT('Ctrl Pts',(2.15658940161914,-24.38545599446,13.5097021066617));
#5473=CARTESIAN_POINT('Ctrl Pts',(1.16899629669851,-23.8324631397826,13.3969816589274));
#5474=CARTESIAN_POINT('Ctrl Pts',(0.595873591284971,-23.6759518953122,13.3384105505808));
#5475=CARTESIAN_POINT('Ctrl Pts',(-0.542597791496814,-23.6538565319805,
13.2256821461812));
#5476=CARTESIAN_POINT('Ctrl Pts',(-1.12522575253909,-23.7868779724016,13.1671166510507));
#5477=CARTESIAN_POINT('Ctrl Pts',(-2.14566801741853,-24.3073211065181,13.0543803577285));
#5478=CARTESIAN_POINT('Ctrl Pts',(-2.59937638691691,-24.701666617617,12.9958204257171));
#5479=CARTESIAN_POINT('Ctrl Pts',(-3.25773378013043,-25.6473839761436,12.8830763103964));
#5480=CARTESIAN_POINT('Ctrl Pts',(-3.47313043910005,-26.212360571083,12.8245218920592));
#5481=CARTESIAN_POINT('Ctrl Pts',(-3.60855894375147,-27.3635431571582,12.7117700208398));
#5482=CARTESIAN_POINT('Ctrl Pts',(-3.53164820596563,-27.9668164001819,12.653221067429));
#5483=CARTESIAN_POINT('Ctrl Pts',(-3.105767091041,-29.0521864280927,12.5404615055064));
#5484=CARTESIAN_POINT('Ctrl Pts',(-2.75143959109056,-29.55077490875,12.4819179689183));
#5485=CARTESIAN_POINT('Ctrl Pts',(-1.85890580402603,-30.3115120597038,12.3691507807721));
#5486=CARTESIAN_POINT('Ctrl Pts',(-1.3081945297878,-30.5856746334636,12.3106126135393));
#5487=CARTESIAN_POINT('Ctrl Pts',(-0.155746111134357,-30.8371286739892,
12.1978378627637));
#5488=CARTESIAN_POINT('Ctrl Pts',(0.462685804992595,-30.8191132063823,12.139305018059));
#5489=CARTESIAN_POINT('Ctrl Pts',(1.60409817929837,-30.4955898274631,12.0265227675285));
#5490=CARTESIAN_POINT('Ctrl Pts',(2.14401353900223,-30.1863430662765,11.9679951991224));
#5491=CARTESIAN_POINT('Ctrl Pts',(3.0029277807162,-29.3581080838186,11.8552055109129));
#5492=CARTESIAN_POINT('Ctrl Pts',(3.33509494434164,-28.8278329751593,11.7966831731882));
#5493=CARTESIAN_POINT('Ctrl Pts',(3.70409561193239,-27.685967468371,11.683886108631));
#5494=CARTESIAN_POINT('Ctrl Pts',(3.74721495187959,-27.0582119442714,11.625368956566));
#5495=CARTESIAN_POINT('Ctrl Pts',(3.53299608505888,-25.870552787456,11.5125645762306));
#5496=CARTESIAN_POINT('Ctrl Pts',(3.2735736115038,-25.2934299085353,11.4540525653972));
#5497=CARTESIAN_POINT('Ctrl Pts',(2.52042869786703,-24.3417489691358,11.3412409291145));
#5498=CARTESIAN_POINT('Ctrl Pts',(2.01674443178381,-23.9529912521879,11.2827340156484));
#5499=CARTESIAN_POINT('Ctrl Pts',(0.897592673462909,-23.4661470211606,11.1699151825515));
#5500=CARTESIAN_POINT('Ctrl Pts',(0.266642069111921,-23.3602399484491,11.1114133231524));
#5501=CARTESIAN_POINT('Ctrl Pts',(-1.39312403049024,-23.4944565581067,10.958329580206));
#5502=CARTESIAN_POINT('Ctrl Pts',(-2.41058934284747,-24.0479122951631,10.85928810599));
#5503=CARTESIAN_POINT('Ctrl Pts',(-3.38012308207534,-25.3235402607357,10.7121475096328));
#5504=CARTESIAN_POINT('Ctrl Pts',(-3.61045637172483,-25.8164315543238,10.6637138260613));
#5505=CARTESIAN_POINT('Ctrl Pts',(-3.79323377757728,-26.601419153468,10.5898967883847));
#5506=CARTESIAN_POINT('Ctrl Pts',(-3.82680255063948,-26.8694387362392,10.5653656805807));
#5507=CARTESIAN_POINT('Ctrl Pts',(-3.83622987000688,-27.4039427802795,10.5170549441175));
#5508=CARTESIAN_POINT('Ctrl Pts',(-3.81325471757559,-27.7633704519633,10.4924002112853));
#5509=CARTESIAN_POINT('Ctrl Pts',(-3.79839227204515,-28.1037804107033,10.4678560893805));
#5510=CARTESIAN_POINT('Ctrl Pts',(-2.50007468964084,-27.2248755616029,22.496222040721));
#5511=CARTESIAN_POINT('Ctrl Pts',(-2.4973242723684,-27.6307151961139,22.4400341067123));
#5512=CARTESIAN_POINT('Ctrl Pts',(-2.39007159429291,-28.046172113602,22.3812276634974));
#5513=CARTESIAN_POINT('Ctrl Pts',(-1.80411234252432,-29.1254962791506,22.2128972978767));
#5514=CARTESIAN_POINT('Ctrl Pts',(-1.01989852503814,-29.6445405955095,22.0951434327917));
#5515=CARTESIAN_POINT('Ctrl Pts',(0.638659850934362,-29.7975771342655,21.8706442358959));
#5516=CARTESIAN_POINT('Ctrl Pts',(1.52050172618105,-29.4280871251508,21.7529291734536));
#5517=CARTESIAN_POINT('Ctrl Pts',(2.58730375628404,-28.1125755004147,21.5283726421196));
#5518=CARTESIAN_POINT('Ctrl Pts',(2.77328092962595,-27.1587210142988,21.4106954876537));
#5519=CARTESIAN_POINT('Ctrl Pts',(2.26434145573703,-25.5138542577944,21.1860829502175));
#5520=CARTESIAN_POINT('Ctrl Pts',(1.56361535497179,-24.8180418564626,21.0684428391104));
#5521=CARTESIAN_POINT('Ctrl Pts',(-0.113578182603178,-24.3188792204675,
20.8437755788229));
#5522=CARTESIAN_POINT('Ctrl Pts',(-1.09685694279567,-24.5177986374849,20.726171675136));
#5523=CARTESIAN_POINT('Ctrl Pts',(-2.46562846601663,-25.6525708058311,20.5014509327792));
#5524=CARTESIAN_POINT('Ctrl Pts',(-2.85270323093671,-26.5950681007635,20.383882428069));
#5525=CARTESIAN_POINT('Ctrl Pts',(-2.66720520340355,-28.3915929833279,20.1591094030512));
#5526=CARTESIAN_POINT('Ctrl Pts',(-2.09004397716378,-29.2502097002576,20.0415755151492));
#5527=CARTESIAN_POINT('Ctrl Pts',(-0.468616896601317,-30.1076003596666,
19.8167513681195));
#5528=CARTESIAN_POINT('Ctrl Pts',(0.581634471425745,-30.1049239556306,19.699251339979));
#5529=CARTESIAN_POINT('Ctrl Pts',(2.22026469765585,-29.2201449048687,19.4743771937204));
#5530=CARTESIAN_POINT('Ctrl Pts',(2.81039817593113,-28.3324724230921,19.3569102925241));
#5531=CARTESIAN_POINT('Ctrl Pts',(2.98817389216117,-26.4505314144785,19.1319872339844));
#5532=CARTESIAN_POINT('Ctrl Pts',(2.57213367128736,-25.4521313258754,19.0145527500132));
#5533=CARTESIAN_POINT('Ctrl Pts',(1.08461864343106,-24.2407136856522,18.7895818316129));
#5534=CARTESIAN_POINT('Ctrl Pts',(0.0079989386097899,-24.0287190409257,
18.6721790772003));
#5535=CARTESIAN_POINT('Ctrl Pts',(-1.85262967084505,-24.6003712530939,18.4471613186385));
#5536=CARTESIAN_POINT('Ctrl Pts',(-2.63824608070795,-25.3887272943005,18.3297896275641));
#5537=CARTESIAN_POINT('Ctrl Pts',(-3.20507999580496,-27.2801498666274,18.1047260161945));
#5538=CARTESIAN_POINT('Ctrl Pts',(-2.9831661840297,-28.3867601727525,17.9873847427204));
#5539=CARTESIAN_POINT('Ctrl Pts',(-1.70784482643357,-29.9307658723301,17.7622762360219));
#5540=CARTESIAN_POINT('Ctrl Pts',(-0.650030706902046,-30.3672083689872,
17.644964753788));
#5541=CARTESIAN_POINT('Ctrl Pts',(0.86517973525876,-30.2134209812991,17.4761003984285));
#5542=CARTESIAN_POINT('Ctrl Pts',(1.36724950404345,-30.0318411970833,17.4174556663687));
#5543=CARTESIAN_POINT('Ctrl Pts',(2.21565635117443,-29.4614074155449,17.3048686073546));
#5544=CARTESIAN_POINT('Ctrl Pts',(2.57530040105309,-29.0619448951219,17.2462310962596));
#5545=CARTESIAN_POINT('Ctrl Pts',(3.05799696942356,-28.1527778895029,17.1336333259815));
#5546=CARTESIAN_POINT('Ctrl Pts',(3.18778444768463,-27.6274550492092,17.0750029627851));
#5547=CARTESIAN_POINT('Ctrl Pts',(3.18497660068733,-26.5910853699601,16.962394590283));
#5548=CARTESIAN_POINT('Ctrl Pts',(3.05096346769537,-26.0630986912955,16.9037713029446));
#5549=CARTESIAN_POINT('Ctrl Pts',(2.5567008235024,-25.1442072778572,16.7911524358858));
#5550=CARTESIAN_POINT('Ctrl Pts',(2.1872241769026,-24.739037088108,16.7325361534412));
#5551=CARTESIAN_POINT('Ctrl Pts',(1.31236770377724,-24.1576871529312,16.6199068976086));
#5552=CARTESIAN_POINT('Ctrl Pts',(0.792135943566477,-23.9732771310202,16.5612975501836));
#5553=CARTESIAN_POINT('Ctrl Pts',(-0.260437820231423,-23.8722213494922,
16.4486580099836));
#5554=CARTESIAN_POINT('Ctrl Pts',(-0.809748106445171,-23.9553144054265,
16.390055528683));
#5555=CARTESIAN_POINT('Ctrl Pts',(-1.79217761419359,-24.3649921488181,16.2774058068813));
#5556=CARTESIAN_POINT('Ctrl Pts',(-2.24037789826756,-24.6993373233115,16.218810123806));
#5557=CARTESIAN_POINT('Ctrl Pts',(-2.91818319073377,-25.5291330491587,16.1061503217773));
#5558=CARTESIAN_POINT('Ctrl Pts',(-3.15742799488839,-26.0385267016838,16.0475613699998));
#5559=CARTESIAN_POINT('Ctrl Pts',(-3.36546916479862,-27.0967208098436,15.9348915875478));
#5560=CARTESIAN_POINT('Ctrl Pts',(-3.33619712510802,-27.6623520759774,15.8763093011718));
#5561=CARTESIAN_POINT('Ctrl Pts',(-3.01887153431984,-28.7003948804001,15.7636296366105));
#5562=CARTESIAN_POINT('Ctrl Pts',(-2.72459468751986,-29.1885528069202,15.7050539506644));
#5563=CARTESIAN_POINT('Ctrl Pts',(-1.95049695499757,-29.9594426420382,15.5923645009688));
#5564=CARTESIAN_POINT('Ctrl Pts',(-1.45777472744879,-30.2531246134102,15.5337953513482));
#5565=CARTESIAN_POINT('Ctrl Pts',(-0.404996203962134,-30.5701788649903,
15.4210962121377));
#5566=CARTESIAN_POINT('Ctrl Pts',(0.171589539965396,-30.5971282455161,15.3625335357178));
#5567=CARTESIAN_POINT('Ctrl Pts',(1.2564041637795,-30.3791641241848,15.2498248010666));
#5568=CARTESIAN_POINT('Ctrl Pts',(1.7808885766526,-30.1296197230846,15.191268535602));
#5569=CARTESIAN_POINT('Ctrl Pts',(2.64032159058155,-29.4216164413268,15.0785502984466));
#5570=CARTESIAN_POINT('Ctrl Pts',(2.98741885003,-28.9514201645629,15.020000382554));
#5571=CARTESIAN_POINT('Ctrl Pts',(3.41436167748328,-27.9154309228547,14.9072727343391));
#5572=CARTESIAN_POINT('Ctrl Pts',(3.49938894615047,-27.33357014347,14.8487291075262));
#5573=CARTESIAN_POINT('Ctrl Pts',(3.38693228948582,-26.2116677322755,14.7359921385168));
#5574=CARTESIAN_POINT('Ctrl Pts',(3.18644926086099,-25.6550219465471,14.6774547411401));
#5575=CARTESIAN_POINT('Ctrl Pts',(2.55456776253514,-24.7127415137188,14.5647085402118));
#5576=CARTESIAN_POINT('Ctrl Pts',(2.11270614385815,-24.3138825519738,14.5061773134232));
#5577=CARTESIAN_POINT('Ctrl Pts',(1.10509623772621,-23.7773739118781,14.3934219683943));
#5578=CARTESIAN_POINT('Ctrl Pts',(0.523896870543996,-23.6329943635978,14.3348968541539));
#5579=CARTESIAN_POINT('Ctrl Pts',(-0.624652737702608,-23.6347588544248,
14.2221324514446));
#5580=CARTESIAN_POINT('Ctrl Pts',(-1.20879247712363,-23.7822469180229,14.1636133925763));
#5581=CARTESIAN_POINT('Ctrl Pts',(-2.22710033309911,-24.3284757709235,14.0508400174531));
#5582=CARTESIAN_POINT('Ctrl Pts',(-2.67543546793117,-24.7363080687151,13.9923269575302));
#5583=CARTESIAN_POINT('Ctrl Pts',(-3.31995572055526,-25.7038593482239,13.8795446941064));
#5584=CARTESIAN_POINT('Ctrl Pts',(-3.52434754507323,-26.278264235651,13.8210375774492));
#5585=CARTESIAN_POINT('Ctrl Pts',(-3.63740938510682,-27.4423610026541,13.7082465087035));
#5586=CARTESIAN_POINT('Ctrl Pts',(-3.54639746864993,-28.0488633044433,13.6497452804224));
#5587=CARTESIAN_POINT('Ctrl Pts',(-3.09473081749969,-29.1352984662438,13.5369454881091));
#5588=CARTESIAN_POINT('Ctrl Pts',(-2.72643980864282,-29.6301994280082,13.478450094058));
#5589=CARTESIAN_POINT('Ctrl Pts',(-1.81058422903492,-30.3799260240416,13.3656416589045));
#5590=CARTESIAN_POINT('Ctrl Pts',(-1.24923928464285,-30.6443497337891,13.3071520456616));
#5591=CARTESIAN_POINT('Ctrl Pts',(-0.0812475223329433,-30.8752422580876,
13.1943350472226));
#5592=CARTESIAN_POINT('Ctrl Pts',(0.542066688264732,-30.8436819845603,13.1358511620963));
#5593=CARTESIAN_POINT('Ctrl Pts',(1.68770676819748,-30.4947449812449,13.023025678902));
#5594=CARTESIAN_POINT('Ctrl Pts',(2.22565295815195,-30.1712562533038,12.964547469888));
#5595=CARTESIAN_POINT('Ctrl Pts',(3.0765239957466,-29.3185568856795,12.8517135793952));
#5596=CARTESIAN_POINT('Ctrl Pts',(3.40033958384053,-28.7766023480984,12.7932409951886));
#5597=CARTESIAN_POINT('Ctrl Pts',(3.75086916774635,-27.6168033809139,12.6803987738176));
#5598=CARTESIAN_POINT('Ctrl Pts',(3.78118157345793,-26.9825964758114,12.6219317637952));
#5599=CARTESIAN_POINT('Ctrl Pts',(3.54228427860331,-25.7876249293633,12.5090812869421));
#5600=CARTESIAN_POINT('Ctrl Pts',(3.26854073808389,-25.210742371226,12.4506198011539));
#5601=CARTESIAN_POINT('Ctrl Pts',(2.49014580888264,-24.2640365549505,12.3377611432072));
#5602=CARTESIAN_POINT('Ctrl Pts',(1.97390729235221,-23.8821408071608,12.2793051323495));
#5603=CARTESIAN_POINT('Ctrl Pts',(0.834700026419599,-23.4114217906921,12.1664383667394));
#5604=CARTESIAN_POINT('Ctrl Pts',(0.195831970432003,-23.3174137365592,12.1079877821605));
#5605=CARTESIAN_POINT('Ctrl Pts',(-1.47788166551791,-23.4836412312721,11.9548377869386));
#5606=CARTESIAN_POINT('Ctrl Pts',(-2.49443750143783,-24.0624257587396,11.8558411914807));
#5607=CARTESIAN_POINT('Ctrl Pts',(-3.44927269813164,-25.3687928546683,11.7087129913786));
#5608=CARTESIAN_POINT('Ctrl Pts',(-3.67294424006971,-25.8708425746013,11.6602623470862));
#5609=CARTESIAN_POINT('Ctrl Pts',(-3.84264085815611,-26.6669511684813,11.5864611273604));
#5610=CARTESIAN_POINT('Ctrl Pts',(-3.8715225401559,-26.9382115207412,11.561931682028));
#5611=CARTESIAN_POINT('Ctrl Pts',(-3.871490282254,-27.4782887242644,11.5136003532919));
#5612=CARTESIAN_POINT('Ctrl Pts',(-3.84967700978782,-27.8368139613051,11.4889556287746));
#5613=CARTESIAN_POINT('Ctrl Pts',(-3.83481456425754,-28.1772239200439,11.4644115068716));
#5614=CARTESIAN_POINT('Ctrl Pts',(-3.49996080530815,-27.2127230666419,22.4975165628198));
#5615=CARTESIAN_POINT('Ctrl Pts',(-3.49923858446785,-27.7853227106402,22.4402329418509));
#5616=CARTESIAN_POINT('Ctrl Pts',(-3.35442400014962,-28.3588108293565,22.3829524076267));
#5617=CARTESIAN_POINT('Ctrl Pts',(-2.53805890913148,-29.8820941336696,22.2111092614391));
#5618=CARTESIAN_POINT('Ctrl Pts',(-1.46143501137141,-30.6017071597437,22.0965431123954));
#5619=CARTESIAN_POINT('Ctrl Pts',(0.859993909463204,-30.8281716102345,21.8674140533199));
#5620=CARTESIAN_POINT('Ctrl Pts',(2.07105132984979,-30.3269875071567,21.7528496294383));
#5621=CARTESIAN_POINT('Ctrl Pts',(3.56717700801455,-28.5011027334814,21.5237158877512));
#5622=CARTESIAN_POINT('Ctrl Pts',(3.82655802944863,-27.2003585446699,21.4091531369767));
#5623=CARTESIAN_POINT('Ctrl Pts',(3.13176866916735,-24.9149704304093,21.1800148858282));
#5624=CARTESIAN_POINT('Ctrl Pts',(2.18340277243941,-23.9654078612039,21.0654537578317));
#5625=CARTESIAN_POINT('Ctrl Pts',(-0.129624475723444,-23.26492626726,20.8363111624828));
#5626=CARTESIAN_POINT('Ctrl Pts',(-1.46146161962901,-23.5287714044906,20.7217516085899));
#5627=CARTESIAN_POINT('Ctrl Pts',(-3.35087032746474,-25.0803824700087,20.4926048268444));
#5628=CARTESIAN_POINT('Ctrl Pts',(-3.87760724316326,-26.3487572317876,20.3780467999886));
#5629=CARTESIAN_POINT('Ctrl Pts',(-3.63476056023195,-28.8097599072106,20.1488959825923));
#5630=CARTESIAN_POINT('Ctrl Pts',(-2.86424004281594,-29.965541294796,20.0343394372402));
#5631=CARTESIAN_POINT('Ctrl Pts',(-0.658453525508203,-31.1444028451946,
19.8051847283177));
#5632=CARTESIAN_POINT('Ctrl Pts',(0.746295607863299,-31.1460497722331,19.6906296204221));
#5633=CARTESIAN_POINT('Ctrl Pts',(2.97686521751534,-29.9539838567283,19.4614711577696));
#5634=CARTESIAN_POINT('Ctrl Pts',(3.76753534062837,-28.7739677375461,19.3469174447372));
#5635=CARTESIAN_POINT('Ctrl Pts',(4.01866309430747,-26.2291292657398,19.1177553601879));
#5636=CARTESIAN_POINT('Ctrl Pts',(3.47096346939119,-24.9015823386939,19.0032030007967));
#5637=CARTESIAN_POINT('Ctrl Pts',(1.47301680764982,-23.2609008561182,18.7740374205694));
#5638=CARTESIAN_POINT('Ctrl Pts',(0.0495864900580295,-22.9755165719832,
18.6594863749187));
#5639=CARTESIAN_POINT('Ctrl Pts',(-2.45153366210842,-23.7331018039879,18.4303174198824));
#5640=CARTESIAN_POINT('Ctrl Pts',(-3.49083915992615,-24.7690401632385,18.3157676493834));
#5641=CARTESIAN_POINT('Ctrl Pts',(-4.25889868811986,-27.2963083875918,18.0865954352922));
#5642=CARTESIAN_POINT('Ctrl Pts',(-3.97206991737307,-28.7513902818761,17.9720469025882));
#5643=CARTESIAN_POINT('Ctrl Pts',(-2.27985145267618,-30.8159510369377,17.7428715404485));
#5644=CARTESIAN_POINT('Ctrl Pts',(-0.896239671425334,-31.3920117915409,
17.6283242093665));
#5645=CARTESIAN_POINT('Ctrl Pts',(1.11729400206607,-31.1951401445063,17.4564404065291));
#5646=CARTESIAN_POINT('Ctrl Pts',(1.77292736544793,-30.9607175289896,17.3991671837723));
#5647=CARTESIAN_POINT('Ctrl Pts',(2.90077819546148,-30.2083455155492,17.2845772407366));
#5648=CARTESIAN_POINT('Ctrl Pts',(3.37094068270095,-29.6898924273955,17.2273043052763));
#5649=CARTESIAN_POINT('Ctrl Pts',(4.01431528178035,-28.4885418055165,17.1127136336125));
#5650=CARTESIAN_POINT('Ctrl Pts',(4.18547814755316,-27.8061836720571,17.0554409812454));
#5651=CARTESIAN_POINT('Ctrl Pts',(4.18663754642286,-26.4363906879155,16.9408495931827));
#5652=CARTESIAN_POINT('Ctrl Pts',(4.0150884896742,-25.7504104196397,16.8835772197774));
#5653=CARTESIAN_POINT('Ctrl Pts',(3.36714801944677,-24.5356000655517,16.7689851273202));
#5654=CARTESIAN_POINT('Ctrl Pts',(2.89009172502227,-24.0087892511978,16.7117130288065));
#5655=CARTESIAN_POINT('Ctrl Pts',(1.7402086697919,-23.2389101700822,16.5971202437039));
#5656=CARTESIAN_POINT('Ctrl Pts',(1.06776209555002,-22.9979372337308,16.5398484160816));
#5657=CARTESIAN_POINT('Ctrl Pts',(-0.31623274086958,-22.8602643582168,16.4252549498493));
#5658=CARTESIAN_POINT('Ctrl Pts',(-1.02644456351773,-22.9652272065363,16.3679833891743));
#5659=CARTESIAN_POINT('Ctrl Pts',(-2.31841804031954,-23.4988447092972,16.2533892531115));
#5660=CARTESIAN_POINT('Ctrl Pts',(-2.8982081868341,-23.9283243595328,16.1961179554988));
#5661=CARTESIAN_POINT('Ctrl Pts',(-3.79057690805528,-25.0133430809505,16.0815231606726));
#5662=CARTESIAN_POINT('Ctrl Pts',(-4.10102526300207,-25.6686660718134,16.024252122308));
#5663=CARTESIAN_POINT('Ctrl Pts',(-4.37797862822859,-27.0530885949626,15.909656679556));
#5664=CARTESIAN_POINT('Ctrl Pts',(-4.34271119481323,-27.7809795875592,15.8523858966855));
#5665=CARTESIAN_POINT('Ctrl Pts',(-3.93237495733071,-29.1392105157473,15.7377898166423));
#5666=CARTESIAN_POINT('Ctrl Pts',(-3.55632299466167,-29.7676390000464,15.6805192855666));
#5667=CARTESIAN_POINT('Ctrl Pts',(-2.54926136464863,-30.7770591329649,15.5659225786565));
#5668=CARTESIAN_POINT('Ctrl Pts',(-1.91829944896927,-31.1558975036044,15.5086522957306));
#5669=CARTESIAN_POINT('Ctrl Pts',(-0.547625232561448,-31.5734932671083,
15.3940549721839));
#5670=CARTESIAN_POINT('Ctrl Pts',(0.191015893047531,-31.6103769951178,15.3367849338207));
#5671=CARTESIAN_POINT('Ctrl Pts',(1.60357971999462,-31.3312243440256,15.222187003658));
#5672=CARTESIAN_POINT('Ctrl Pts',(2.27566348949658,-31.0140495365735,15.1649172063298));
#5673=CARTESIAN_POINT('Ctrl Pts',(3.39529563646339,-30.0975823003571,15.0503186793825));
#5674=CARTESIAN_POINT('Ctrl Pts',(3.84068011604263,-29.498165831456,14.9930491196166));
#5675=CARTESIAN_POINT('Ctrl Pts',(4.39882341638518,-28.1556730779471,14.8784500055221));
#5676=CARTESIAN_POINT('Ctrl Pts',(4.50961669585736,-27.4135215250066,14.8211806798972));
#5677=CARTESIAN_POINT('Ctrl Pts',(4.36838003559756,-25.9594643878227,14.706580988118));
#5678=CARTESIAN_POINT('Ctrl Pts',(4.11506029041641,-25.249312658991,14.64931189327));
#5679=CARTESIAN_POINT('Ctrl Pts',(3.30121940653211,-24.0276707334375,14.5347116330704));
#5680=CARTESIAN_POINT('Ctrl Pts',(2.74039982125199,-23.5183420501783,14.4774427656859));
#5681=CARTESIAN_POINT('Ctrl Pts',(1.44062797695419,-22.8212395033473,14.3628419461743));
#5682=CARTESIAN_POINT('Ctrl Pts',(0.702445412717409,-22.6355127980759,14.3055733029845));
#5683=CARTESIAN_POINT('Ctrl Pts',(-0.779466818671152,-22.6333745501127,
14.1909719330902));
#5684=CARTESIAN_POINT('Ctrl Pts',(-1.52154027083034,-22.8183992461163,14.133703510881));
#5685=CARTESIAN_POINT('Ctrl Pts',(-2.83568124304263,-23.5183337811168,14.0191015993632));
#5686=CARTESIAN_POINT('Ctrl Pts',(-3.40560315083273,-24.0337181522913,13.961833394971));
#5687=CARTESIAN_POINT('Ctrl Pts',(-4.23856228598614,-25.2762788645662,13.8472309504247));
#5688=CARTESIAN_POINT('Ctrl Pts',(-4.49948190557238,-26.0028485522343,13.789962960732));
#5689=CARTESIAN_POINT('Ctrl Pts',(-4.6490886604143,-27.4983069550493,13.6753599915962));
#5690=CARTESIAN_POINT('Ctrl Pts',(-4.53619916170288,-28.2656495705488,13.6180922135344));
#5691=CARTESIAN_POINT('Ctrl Pts',(-3.96055736820013,-29.661540425932,13.5034887280845));
#5692=CARTESIAN_POINT('Ctrl Pts',(-3.49715379610915,-30.2879729181394,13.4462211586326));
#5693=CARTESIAN_POINT('Ctrl Pts',(-2.32608670582391,-31.2521669466145,13.3316171649959));
#5694=CARTESIAN_POINT('Ctrl Pts',(-1.61885949052411,-31.5877524818146,13.2743498011764));
#5695=CARTESIAN_POINT('Ctrl Pts',(-0.124696310905245,-31.8874771910156,
13.1597453073302));
#5696=CARTESIAN_POINT('Ctrl Pts',(0.660815950487942,-31.8499065009576,13.1024781462114));
#5697=CARTESIAN_POINT('Ctrl Pts',(2.12655441499977,-31.4079152525417,12.9878731599857));
#5698=CARTESIAN_POINT('Ctrl Pts',(2.80470906709709,-31.0026671109796,12.9306061986817));
#5699=CARTESIAN_POINT('Ctrl Pts',(3.89400923429049,-29.9170086021089,12.8160007277616));
#5700=CARTESIAN_POINT('Ctrl Pts',(4.30293326762064,-29.2368576811396,12.7587339634332));
#5701=CARTESIAN_POINT('Ctrl Pts',(4.7539165316201,-27.7592163768989,12.6441280153592));
#5702=CARTESIAN_POINT('Ctrl Pts',(4.79414098254103,-26.9630153236094,12.5868614452008));
#5703=CARTESIAN_POINT('Ctrl Pts',(4.49400280036036,-25.4403847040206,12.4722550273998));
#5704=CARTESIAN_POINT('Ctrl Pts',(4.15263788850493,-24.7159678807397,12.4149886486516));
#5705=CARTESIAN_POINT('Ctrl Pts',(3.16577605609634,-23.509168568218,12.3003817683865));
#5706=CARTESIAN_POINT('Ctrl Pts',(2.52035612956819,-23.0290393182234,12.2431155783337));
#5707=CARTESIAN_POINT('Ctrl Pts',(1.07469387470518,-22.4272153063553,12.1285082427589));
#5708=CARTESIAN_POINT('Ctrl Pts',(0.275594950052222,-22.3074707664612,12.0712422387231));
#5709=CARTESIAN_POINT('Ctrl Pts',(-1.84866925673703,-22.5128307999096,11.915740909639));
#5710=CARTESIAN_POINT('Ctrl Pts',(-3.12603843365803,-23.2394090136764,11.8175868796768));
#5711=CARTESIAN_POINT('Ctrl Pts',(-4.3320981071104,-24.8804056714019,11.6703283443192));
#5712=CARTESIAN_POINT('Ctrl Pts',(-4.61674384788206,-25.5146057311216,11.6212316068295));
#5713=CARTESIAN_POINT('Ctrl Pts',(-4.83246869871424,-26.5137556598953,11.5476071541803));
#5714=CARTESIAN_POINT('Ctrl Pts',(-4.86977624768409,-26.8545749239038,11.5230638633071));
#5715=CARTESIAN_POINT('Ctrl Pts',(-4.87146626433893,-27.5373932865771,11.4739653075255));
#5716=CARTESIAN_POINT('Ctrl Pts',(-4.84802535953691,-27.8775521427343,11.449426192242));
#5717=CARTESIAN_POINT('Ctrl Pts',(-4.83316291400662,-28.2179621014742,11.4248820703399));
#5718=CARTESIAN_POINT('Origin',(-3.5,-27.1629509039024,22.));
#5719=CARTESIAN_POINT('Origin',(-3.5,-27.1629509039024,22.));
#5720=CARTESIAN_POINT('',(0.,0.,0.));
#5721=CARTESIAN_POINT('Origin',(0.,0.,2.));
#5722=CARTESIAN_POINT('',(-2.65,-3.24531401774049E-16,0.));
#5723=CARTESIAN_POINT('Origin',(0.,0.,0.));
#5724=CARTESIAN_POINT('',(-2.65,-3.24531401774049E-16,2.));
#5725=CARTESIAN_POINT('',(-2.65,-3.24531401774049E-16,2.));
#5726=CARTESIAN_POINT('Origin',(0.,0.,2.));
#5727=CARTESIAN_POINT('Origin',(16.1421356237309,-27.1629509039023,0.));
#5728=CARTESIAN_POINT('',(8.14213562373088,-27.1629509039023,-2.5));
#5729=CARTESIAN_POINT('Origin',(8.14213562373088,-27.1629509039023,0.));
#5730=CARTESIAN_POINT('',(16.1421356237309,-27.1629509039023,-2.5));
#5731=CARTESIAN_POINT('',(16.1421356237309,-27.1629509039023,-2.5));
#5732=CARTESIAN_POINT('',(16.1421356237309,-29.6629509039023,0.));
#5733=CARTESIAN_POINT('Origin',(16.1421356237309,-27.1629509039023,0.));
#5734=CARTESIAN_POINT('',(12.1421356237309,-29.6629509039023,0.));
#5735=CARTESIAN_POINT('',(16.1421356237309,-29.6629509039023,0.));
#5736=CARTESIAN_POINT('',(12.1421356237309,-28.6629509039023,2.));
#5737=CARTESIAN_POINT('Origin',(12.1421356237309,-27.1629509039023,0.));
#5738=CARTESIAN_POINT('',(16.1421356237309,-28.6629509039023,2.));
#5739=CARTESIAN_POINT('',(16.1421356237309,-28.6629509039023,2.));
#5740=CARTESIAN_POINT('',(16.1421356237309,-25.6629509039023,2.));
#5741=CARTESIAN_POINT('Origin',(16.1421356237309,-27.1629509039023,0.));
#5742=CARTESIAN_POINT('',(12.1421356237309,-25.6629509039023,2.));
#5743=CARTESIAN_POINT('',(16.1421356237309,-25.6629509039023,2.));
#5744=CARTESIAN_POINT('',(12.1421356237309,-24.6629509039023,0.));
#5745=CARTESIAN_POINT('Origin',(12.1421356237309,-27.1629509039023,0.));
#5746=CARTESIAN_POINT('',(16.1421356237309,-24.6629509039023,0.));
#5747=CARTESIAN_POINT('',(16.1421356237309,-24.6629509039023,0.));
#5748=CARTESIAN_POINT('Origin',(16.1421356237309,-27.1629509039023,0.));
#5749=CARTESIAN_POINT('Origin',(12.1421356237309,-18.2842712474619,0.));
#5750=CARTESIAN_POINT('',(12.1421356237309,-64.142135623731,0.));
#5751=CARTESIAN_POINT('',(12.1421356237309,-18.2842712474619,0.));
#5752=CARTESIAN_POINT('',(12.1421356237309,-64.142135623731,2.));
#5753=CARTESIAN_POINT('',(12.1421356237309,-64.142135623731,0.));
#5754=CARTESIAN_POINT('',(12.1421356237309,-18.2842712474619,2.));
#5755=CARTESIAN_POINT('Origin',(5.,0.,2.));
#5756=CARTESIAN_POINT('',(5.,0.,0.));
#5757=CARTESIAN_POINT('',(5.,51.6435909019114,0.));
#5758=CARTESIAN_POINT('',(5.,0.,0.));
#5759=CARTESIAN_POINT('',(5.,51.6435909019114,2.));
#5760=CARTESIAN_POINT('',(5.,51.6435909019114,2.));
#5761=CARTESIAN_POINT('',(5.,0.,2.));
#5762=CARTESIAN_POINT('',(5.,0.,2.));
#5763=CARTESIAN_POINT('',(5.,0.,2.));
#5764=CARTESIAN_POINT('Origin',(-5.,80.,2.));
#5765=CARTESIAN_POINT('',(-2.,80.,0.));
#5766=CARTESIAN_POINT('',(-4.33680868994202E-15,80.,0.));
#5767=CARTESIAN_POINT('',(-5.,80.,0.));
#5768=CARTESIAN_POINT('',(-4.33680868994202E-15,80.,1.15262767247211));
#5769=CARTESIAN_POINT('',(-3.38677286419691,80.,-0.799216389353386));
#5770=CARTESIAN_POINT('',(-4.33680868994202E-15,80.,0.));
#5771=CARTESIAN_POINT('Origin',(-5.,0.,2.));
#5772=CARTESIAN_POINT('',(-5.,0.,1.0373649052249));
#5773=CARTESIAN_POINT('',(-5.,0.,0.));
#5774=CARTESIAN_POINT('',(-5.,0.,2.));
#5775=CARTESIAN_POINT('',(-5.,30.,0.));
#5776=CARTESIAN_POINT('',(-5.,-0.0332470421233885,1.03851454904828));
#5777=CARTESIAN_POINT('',(-5.,0.,0.));
#5778=CARTESIAN_POINT('Origin',(0.,0.,2.));
#5779=CARTESIAN_POINT('',(16.1421356237309,0.,2.));
#5780=CARTESIAN_POINT('',(19.1421356237309,-64.142135623731,2.));
#5781=CARTESIAN_POINT('',(9.14213562373088,-64.142135623731,2.));
#5782=CARTESIAN_POINT('',(19.1421356237309,-14.142135623731,2.));
#5783=CARTESIAN_POINT('',(19.1421356237309,-14.142135623731,2.));
#5784=CARTESIAN_POINT('',(5.,0.,2.));
#5785=CARTESIAN_POINT('',(1.09703553512821,73.7784023141528,2.));
#5786=CARTESIAN_POINT('',(-4.33680868994202E-15,80.,2.));
#5787=CARTESIAN_POINT('',(-3.44991431960659,-2.00409526476049,2.));
#5788=CARTESIAN_POINT('',(-1.54211698258366,29.792527018955,2.));
#5789=CARTESIAN_POINT('',(12.1421356237309,-22.1629509039023,2.));
#5790=CARTESIAN_POINT('',(-5.,0.,2.));
#5791=CARTESIAN_POINT('',(12.1421356237309,-18.2842712474619,2.));
#5792=CARTESIAN_POINT('Origin',(0.,0.,0.));
#5793=CARTESIAN_POINT('',(16.1421356237309,0.,0.));
#5794=CARTESIAN_POINT('',(12.1421356237309,-22.1629509039023,0.));
#5795=CARTESIAN_POINT('',(12.1421356237309,-18.2842712474619,0.));
#5796=CARTESIAN_POINT('',(-5.,0.,0.));
#5797=CARTESIAN_POINT('',(-6.77560781187724,0.406536468712635,0.));
#5798=CARTESIAN_POINT('',(13.6808057330267,2.41229516856365,0.));
#5799=CARTESIAN_POINT('',(19.1421356237309,-14.142135623731,0.));
#5800=CARTESIAN_POINT('',(5.,0.,0.));
#5801=CARTESIAN_POINT('',(19.1421356237309,-64.142135623731,0.));
#5802=CARTESIAN_POINT('',(19.1421356237309,-14.142135623731,0.));
#5803=CARTESIAN_POINT('',(9.14213562373088,-64.142135623731,0.));
#5804=CARTESIAN_POINT('Origin',(-5.,0.,0.));
#5805=CARTESIAN_POINT('',(-5.21072112990534,0.272439919915319,0.906502748749744));
#5806=CARTESIAN_POINT('',(12.1421356237309,-22.1629509039023,0.));
#5807=CARTESIAN_POINT('Origin',(5.,0.,0.));
#5808=CARTESIAN_POINT('',(19.1421356237309,-14.142135623731,0.));
#5809=CARTESIAN_POINT('Origin',(19.1421356237309,-14.142135623731,0.));
#5810=CARTESIAN_POINT('',(19.1421356237309,-64.142135623731,0.));
#5811=CARTESIAN_POINT('Origin',(9.14213562373088,-64.142135623731,0.));
#5812=CARTESIAN_POINT('Origin',(12.1421356237309,-18.2842712474619,0.));
#5813=CARTESIAN_POINT('Origin',(-4.33680868994202E-15,80.,2.));
#5814=CARTESIAN_POINT('',(0.019387620776991,79.8900473387618,1.16760306097774));
#5815=CARTESIAN_POINT('Origin',(-3.3177247944609,0.199063487667654,2.));
#5816=CARTESIAN_POINT('Origin',(16.1421356237309,-27.1629509039023,0.));
#5817=CARTESIAN_POINT('Origin',(8.14213562373088,-27.1629509039023,0.));
#5818=CARTESIAN_POINT('Origin',(16.1421356237309,-27.1629509039023,0.));
#5819=CARTESIAN_POINT('',(0.,0.,0.));
#5820=CARTESIAN_POINT('Origin',(15.6421356237309,-34.142135623731,0.));
#5821=CARTESIAN_POINT('',(9.64213562373089,-134.142135623731,-7.34788079488412E-16));
#5822=CARTESIAN_POINT('Origin',(15.6421356237309,-134.142135623731,0.));
#5823=CARTESIAN_POINT('',(9.64213562373088,-34.142135623731,-7.34788079488412E-16));
#5824=CARTESIAN_POINT('',(9.64213562373088,-34.142135623731,-7.34788079488412E-16));
#5825=CARTESIAN_POINT('Origin',(15.6421356237309,-34.142135623731,0.));
#5826=CARTESIAN_POINT('Origin',(15.6421356237309,-134.142135623731,0.));
#5827=CARTESIAN_POINT('Origin',(15.6421356237309,-34.142135623731,0.));
#5828=CARTESIAN_POINT('',(12.1421356237309,-34.142135623731,2.));
#5829=CARTESIAN_POINT('',(19.1421356237309,-34.142135623731,2.));
#5830=CARTESIAN_POINT('',(15.6421356237309,-34.142135623731,2.));
#5831=CARTESIAN_POINT('',(12.1421356237309,-34.142135623731,0.));
#5832=CARTESIAN_POINT('',(12.1421356237309,-34.142135623731,0.));
#5833=CARTESIAN_POINT('',(19.1421356237309,-34.142135623731,0.));
#5834=CARTESIAN_POINT('',(15.6421356237309,-34.142135623731,0.));
#5835=CARTESIAN_POINT('',(19.1421356237309,-34.142135623731,0.));
#5836=CARTESIAN_POINT('Origin',(12.1421356237309,-18.2842712474619,0.));
#5837=CARTESIAN_POINT('',(12.1421356237309,-64.142135623731,2.));
#5838=CARTESIAN_POINT('',(12.1421356237309,-18.2842712474619,2.));
#5839=CARTESIAN_POINT('',(12.1421356237309,-64.142135623731,0.));
#5840=CARTESIAN_POINT('',(12.1421356237309,-64.142135623731,0.));
#5841=CARTESIAN_POINT('',(12.1421356237309,-18.2842712474619,0.));
#5842=CARTESIAN_POINT('Origin',(0.,0.,2.));
#5843=CARTESIAN_POINT('',(19.1421356237309,-64.142135623731,2.));
#5844=CARTESIAN_POINT('',(19.1421356237309,-14.142135623731,2.));
#5845=CARTESIAN_POINT('',(9.14213562373088,-64.142135623731,2.));
#5846=CARTESIAN_POINT('Origin',(0.,0.,0.));
#5847=CARTESIAN_POINT('',(19.1421356237309,-64.142135623731,0.));
#5848=CARTESIAN_POINT('',(9.14213562373088,-64.142135623731,0.));
#5849=CARTESIAN_POINT('',(19.1421356237309,-14.142135623731,0.));
#5850=CARTESIAN_POINT('Origin',(19.1421356237309,-14.142135623731,0.));
#5851=CARTESIAN_POINT('',(19.1421356237309,-64.142135623731,0.));
#5852=CARTESIAN_POINT('Origin',(9.14213562373088,-64.142135623731,0.));
#5853=CARTESIAN_POINT('',(0.,0.,0.));
#5854=CARTESIAN_POINT('Origin',(11.4999999999999,-32.3205080756888,0.));
#5855=CARTESIAN_POINT('',(5.49999999999991,-32.3205080756888,-7.34788079488412E-16));
#5856=CARTESIAN_POINT('Origin',(11.4999999999999,-32.3205080756888,0.));
#5857=CARTESIAN_POINT('',(5.49999999999992,-132.320508075689,-7.34788079488412E-16));
#5858=CARTESIAN_POINT('',(5.49999999999991,-32.3205080756888,-7.34788079488412E-16));
#5859=CARTESIAN_POINT('Origin',(11.4999999999999,-132.320508075689,0.));
#5860=CARTESIAN_POINT('Origin',(11.4999999999999,-32.3205080756888,0.));
#5861=CARTESIAN_POINT('',(4.49999999999992,-133.320508075689,-8.57252759403147E-16));
#5862=CARTESIAN_POINT('Origin',(11.4999999999999,-133.320508075689,0.));
#5863=CARTESIAN_POINT('',(4.49999999999991,-32.3205080756888,-8.57252759403147E-16));
#5864=CARTESIAN_POINT('',(4.49999999999991,-32.3205080756888,-8.57252759403147E-16));
#5865=CARTESIAN_POINT('Origin',(11.4999999999999,-32.3205080756888,0.));
#5866=CARTESIAN_POINT('Origin',(11.4999999999999,-32.3205080756888,0.));
#5867=CARTESIAN_POINT('Origin',(11.4999999999999,-133.320508075689,0.));
#5868=CARTESIAN_POINT('Origin',(11.4999999999999,-132.320508075689,0.));
#5869=CARTESIAN_POINT('',(0.,0.,0.));
#5870=CARTESIAN_POINT('Origin',(0.,0.,4.5));
#5871=CARTESIAN_POINT('',(2.,-2.44929359829471E-16,4.5));
#5872=CARTESIAN_POINT('Origin',(0.,0.,4.5));
#5873=CARTESIAN_POINT('',(2.,-2.44929359829471E-16,2.));
#5874=CARTESIAN_POINT('',(2.,-2.44929359829471E-16,4.5));
#5875=CARTESIAN_POINT('Origin',(0.,0.,2.));
#5876=CARTESIAN_POINT('Origin',(0.,0.,4.5));
#5877=CARTESIAN_POINT('',(4.,-2.3094010767585,4.5));
#5878=CARTESIAN_POINT('',(4.,2.3094010767585,4.5));
#5879=CARTESIAN_POINT('',(4.,-2.3094010767585,4.5));
#5880=CARTESIAN_POINT('',(-1.32814766129474E-15,4.61880215351701,4.5));
#5881=CARTESIAN_POINT('',(4.,2.3094010767585,4.5));
#5882=CARTESIAN_POINT('',(-4.,2.3094010767585,4.5));
#5883=CARTESIAN_POINT('',(-1.32814766129474E-15,4.61880215351701,4.5));
#5884=CARTESIAN_POINT('',(-4.,-2.3094010767585,4.5));
#5885=CARTESIAN_POINT('',(-4.,2.3094010767585,4.5));
#5886=CARTESIAN_POINT('',(3.45589442479754E-15,-4.61880215351701,4.5));
#5887=CARTESIAN_POINT('',(-4.,-2.3094010767585,4.5));
#5888=CARTESIAN_POINT('',(3.45589442479754E-15,-4.61880215351701,4.5));
#5889=CARTESIAN_POINT('Origin',(0.,0.,2.));
#5890=CARTESIAN_POINT('',(4.,-2.3094010767585,2.));
#5891=CARTESIAN_POINT('',(4.,2.3094010767585,2.));
#5892=CARTESIAN_POINT('',(4.,-2.3094010767585,2.));
#5893=CARTESIAN_POINT('',(3.45589442479754E-15,-4.61880215351701,2.));
#5894=CARTESIAN_POINT('',(3.45589442479754E-15,-4.61880215351701,2.));
#5895=CARTESIAN_POINT('',(-4.,-2.3094010767585,2.));
#5896=CARTESIAN_POINT('',(-4.,-2.3094010767585,2.));
#5897=CARTESIAN_POINT('',(-4.,2.3094010767585,2.));
#5898=CARTESIAN_POINT('',(-4.,2.3094010767585,2.));
#5899=CARTESIAN_POINT('',(-1.32814766129474E-15,4.61880215351701,2.));
#5900=CARTESIAN_POINT('',(-1.32814766129474E-15,4.61880215351701,2.));
#5901=CARTESIAN_POINT('',(4.,2.3094010767585,2.));
#5902=CARTESIAN_POINT('Origin',(4.,-2.3094010767585,4.5));
#5903=CARTESIAN_POINT('',(4.,2.3094010767585,4.5));
#5904=CARTESIAN_POINT('',(4.,-2.3094010767585,4.5));
#5905=CARTESIAN_POINT('Origin',(4.,2.3094010767585,4.5));
#5906=CARTESIAN_POINT('',(-1.32814766129474E-15,4.61880215351701,4.5));
#5907=CARTESIAN_POINT('Origin',(-1.32814766129474E-15,4.61880215351701,
4.5));
#5908=CARTESIAN_POINT('',(-4.,2.3094010767585,4.5));
#5909=CARTESIAN_POINT('Origin',(-4.,2.3094010767585,4.5));
#5910=CARTESIAN_POINT('',(-4.,-2.3094010767585,4.5));
#5911=CARTESIAN_POINT('Origin',(-4.,-2.3094010767585,4.5));
#5912=CARTESIAN_POINT('',(3.45589442479754E-15,-4.61880215351701,4.5));
#5913=CARTESIAN_POINT('Origin',(3.45589442479754E-15,-4.61880215351701,
4.5));
#5914=CARTESIAN_POINT('',(0.,0.,0.));
#5915=CARTESIAN_POINT('',(0.,0.,0.));
#5916=CARTESIAN_POINT('',(0.,0.,0.));
#5917=CARTESIAN_POINT('',(0.,0.,0.));
#5918=CARTESIAN_POINT('',(0.,0.,0.));
#5919=CARTESIAN_POINT('',(4.14213562373097,-1.82162754804219,0.));
#5920=CARTESIAN_POINT('',(-11.,0.,0.));
#5921=CARTESIAN_POINT('',(0.,0.,0.));
#5922=CARTESIAN_POINT('',(0.,0.,0.));
#5923=CARTESIAN_POINT('',(-4.14213562373097,-1.82162754804219,0.));
#5924=CARTESIAN_POINT('',(0.,0.,-6.5));
#5925=UNCERTAINTY_MEASURE_WITH_UNIT(LENGTH_MEASURE(0.01),#5943,
'DISTANCE_ACCURACY_VALUE',
'Maximum model space distance between geometric entities at asserted c
onnectivities');
#5926=UNCERTAINTY_MEASURE_WITH_UNIT(LENGTH_MEASURE(0.01),#5943,
'DISTANCE_ACCURACY_VALUE',
'Maximum model space distance between geometric entities at asserted c
onnectivities');
#5927=UNCERTAINTY_MEASURE_WITH_UNIT(LENGTH_MEASURE(0.01),#5943,
'DISTANCE_ACCURACY_VALUE',
'Maximum model space distance between geometric entities at asserted c
onnectivities');
#5928=UNCERTAINTY_MEASURE_WITH_UNIT(LENGTH_MEASURE(0.01),#5943,
'DISTANCE_ACCURACY_VALUE',
'Maximum model space distance between geometric entities at asserted c
onnectivities');
#5929=UNCERTAINTY_MEASURE_WITH_UNIT(LENGTH_MEASURE(0.01),#5943,
'DISTANCE_ACCURACY_VALUE',
'Maximum model space distance between geometric entities at asserted c
onnectivities');
#5930=UNCERTAINTY_MEASURE_WITH_UNIT(LENGTH_MEASURE(0.01),#5943,
'DISTANCE_ACCURACY_VALUE',
'Maximum model space distance between geometric entities at asserted c
onnectivities');
#5931=UNCERTAINTY_MEASURE_WITH_UNIT(LENGTH_MEASURE(0.01),#5943,
'DISTANCE_ACCURACY_VALUE',
'Maximum model space distance between geometric entities at asserted c
onnectivities');
#5932=UNCERTAINTY_MEASURE_WITH_UNIT(LENGTH_MEASURE(0.01),#5943,
'DISTANCE_ACCURACY_VALUE',
'Maximum model space distance between geometric entities at asserted c
onnectivities');
#5933=UNCERTAINTY_MEASURE_WITH_UNIT(LENGTH_MEASURE(0.01),#5943,
'DISTANCE_ACCURACY_VALUE',
'Maximum model space distance between geometric entities at asserted c
onnectivities');
#5934=(
GEOMETRIC_REPRESENTATION_CONTEXT(3)
GLOBAL_UNCERTAINTY_ASSIGNED_CONTEXT((#5925))
GLOBAL_UNIT_ASSIGNED_CONTEXT((#5943,#5945,#5946))
REPRESENTATION_CONTEXT('','3D')
);
#5935=(
GEOMETRIC_REPRESENTATION_CONTEXT(3)
GLOBAL_UNCERTAINTY_ASSIGNED_CONTEXT((#5926))
GLOBAL_UNIT_ASSIGNED_CONTEXT((#5943,#5945,#5946))
REPRESENTATION_CONTEXT('','3D')
);
#5936=(
GEOMETRIC_REPRESENTATION_CONTEXT(3)
GLOBAL_UNCERTAINTY_ASSIGNED_CONTEXT((#5927))
GLOBAL_UNIT_ASSIGNED_CONTEXT((#5943,#5945,#5946))
REPRESENTATION_CONTEXT('','3D')
);
#5937=(
GEOMETRIC_REPRESENTATION_CONTEXT(3)
GLOBAL_UNCERTAINTY_ASSIGNED_CONTEXT((#5928))
GLOBAL_UNIT_ASSIGNED_CONTEXT((#5943,#5945,#5946))
REPRESENTATION_CONTEXT('','3D')
);
#5938=(
GEOMETRIC_REPRESENTATION_CONTEXT(3)
GLOBAL_UNCERTAINTY_ASSIGNED_CONTEXT((#5929))
GLOBAL_UNIT_ASSIGNED_CONTEXT((#5943,#5945,#5946))
REPRESENTATION_CONTEXT('','3D')
);
#5939=(
GEOMETRIC_REPRESENTATION_CONTEXT(3)
GLOBAL_UNCERTAINTY_ASSIGNED_CONTEXT((#5930))
GLOBAL_UNIT_ASSIGNED_CONTEXT((#5943,#5945,#5946))
REPRESENTATION_CONTEXT('','3D')
);
#5940=(
GEOMETRIC_REPRESENTATION_CONTEXT(3)
GLOBAL_UNCERTAINTY_ASSIGNED_CONTEXT((#5931))
GLOBAL_UNIT_ASSIGNED_CONTEXT((#5943,#5945,#5946))
REPRESENTATION_CONTEXT('','3D')
);
#5941=(
GEOMETRIC_REPRESENTATION_CONTEXT(3)
GLOBAL_UNCERTAINTY_ASSIGNED_CONTEXT((#5932))
GLOBAL_UNIT_ASSIGNED_CONTEXT((#5943,#5945,#5946))
REPRESENTATION_CONTEXT('','3D')
);
#5942=(
GEOMETRIC_REPRESENTATION_CONTEXT(3)
GLOBAL_UNCERTAINTY_ASSIGNED_CONTEXT((#5933))
GLOBAL_UNIT_ASSIGNED_CONTEXT((#5943,#5945,#5946))
REPRESENTATION_CONTEXT('','3D')
);
#5943=(
LENGTH_UNIT()
NAMED_UNIT(*)
SI_UNIT(.MILLI.,.METRE.)
);
#5944=(
LENGTH_UNIT()
NAMED_UNIT(*)
SI_UNIT($,.METRE.)
);
#5945=(
NAMED_UNIT(*)
PLANE_ANGLE_UNIT()
SI_UNIT($,.RADIAN.)
);
#5946=(
NAMED_UNIT(*)
SI_UNIT($,.STERADIAN.)
SOLID_ANGLE_UNIT()
);
#5947=SHAPE_DEFINITION_REPRESENTATION(#5955,#5974);
#5948=SHAPE_DEFINITION_REPRESENTATION(#5956,#5975);
#5949=SHAPE_DEFINITION_REPRESENTATION(#5957,#5976);
#5950=SHAPE_DEFINITION_REPRESENTATION(#5958,#5977);
#5951=SHAPE_DEFINITION_REPRESENTATION(#5959,#5978);
#5952=SHAPE_DEFINITION_REPRESENTATION(#5960,#5979);
#5953=SHAPE_DEFINITION_REPRESENTATION(#5961,#5980);
#5954=SHAPE_DEFINITION_REPRESENTATION(#5962,#5981);
#5955=PRODUCT_DEFINITION_SHAPE('',$,#5983);
#5956=PRODUCT_DEFINITION_SHAPE('',$,#5984);
#5957=PRODUCT_DEFINITION_SHAPE('',$,#5985);
#5958=PRODUCT_DEFINITION_SHAPE('',$,#5986);
#5959=PRODUCT_DEFINITION_SHAPE('',$,#5987);
#5960=PRODUCT_DEFINITION_SHAPE('',$,#5988);
#5961=PRODUCT_DEFINITION_SHAPE('',$,#5989);
#5962=PRODUCT_DEFINITION_SHAPE('',$,#5990);
#5963=PRODUCT_DEFINITION_SHAPE($,$,#44);
#5964=PRODUCT_DEFINITION_SHAPE($,$,#45);
#5965=PRODUCT_DEFINITION_SHAPE($,$,#46);
#5966=PRODUCT_DEFINITION_SHAPE($,$,#47);
#5967=PRODUCT_DEFINITION_SHAPE($,$,#48);
#5968=PRODUCT_DEFINITION_SHAPE($,$,#49);
#5969=PRODUCT_DEFINITION_SHAPE($,$,#50);
#5970=PRODUCT_DEFINITION_SHAPE($,$,#51);
#5971=PRODUCT_DEFINITION_SHAPE($,$,#52);
#5972=PRODUCT_DEFINITION_SHAPE($,$,#53);
#5973=PRODUCT_DEFINITION_SHAPE($,$,#54);
#5974=SHAPE_REPRESENTATION('',(#1010,#1100,#1101,#1102,#1103,#1104,#1105,
#1106,#1107,#1108,#1109,#1110),#5934);
#5975=SHAPE_REPRESENTATION('',(#1011),#5935);
#5976=SHAPE_REPRESENTATION('',(#1020),#5936);
#5977=SHAPE_REPRESENTATION('',(#1029),#5937);
#5978=SHAPE_REPRESENTATION('',(#1040),#5938);
#5979=SHAPE_REPRESENTATION('',(#1067),#5939);
#5980=SHAPE_REPRESENTATION('',(#1078),#5940);
#5981=SHAPE_REPRESENTATION('',(#1088),#5941);
#5982=PRODUCT_DEFINITION_CONTEXT('part definition',#6008,'design');
#5983=PRODUCT_DEFINITION('Spring-Loaded Scissors','MAS-152',#5991,#5982);
#5984=PRODUCT_DEFINITION('bushing','bushing',#5992,#5982);
#5985=PRODUCT_DEFINITION('stud','stud',#5993,#5982);
#5986=PRODUCT_DEFINITION('spring','spring',#5994,#5982);
#5987=PRODUCT_DEFINITION('Cutting Blade','Cutting Blade',#5995,#5982);
#5988=PRODUCT_DEFINITION('Forged Aluminum Arm','Forged Aluminum Arm',#5996,
#5982);
#5989=PRODUCT_DEFINITION('Handle Ergonomic Rubber Grip',
'Handle Ergonomic Rubber Grip',#5997,#5982);
#5990=PRODUCT_DEFINITION('lock','lock',#5998,#5982);
#5991=PRODUCT_DEFINITION_FORMATION('',$,#6010);
#5992=PRODUCT_DEFINITION_FORMATION('',$,#6011);
#5993=PRODUCT_DEFINITION_FORMATION('',$,#6012);
#5994=PRODUCT_DEFINITION_FORMATION('',$,#6013);
#5995=PRODUCT_DEFINITION_FORMATION('',$,#6014);
#5996=PRODUCT_DEFINITION_FORMATION('',$,#6015);
#5997=PRODUCT_DEFINITION_FORMATION('',$,#6016);
#5998=PRODUCT_DEFINITION_FORMATION('',$,#6017);
#5999=PRODUCT_RELATED_PRODUCT_CATEGORY('MAS-152','MAS-152',(#6010));
#6000=PRODUCT_RELATED_PRODUCT_CATEGORY('bushing','bushing',(#6011));
#6001=PRODUCT_RELATED_PRODUCT_CATEGORY('stud','stud',(#6012));
#6002=PRODUCT_RELATED_PRODUCT_CATEGORY('spring','spring',(#6013));
#6003=PRODUCT_RELATED_PRODUCT_CATEGORY('Cutting Blade','Cutting Blade',
(#6014));
#6004=PRODUCT_RELATED_PRODUCT_CATEGORY('Forged Aluminum Arm',
'Forged Aluminum Arm',(#6015));
#6005=PRODUCT_RELATED_PRODUCT_CATEGORY('Handle Ergonomic Rubber Grip',
'Handle Ergonomic Rubber Grip',(#6016));
#6006=PRODUCT_RELATED_PRODUCT_CATEGORY('lock','lock',(#6017));
#6007=APPLICATION_PROTOCOL_DEFINITION('international standard',
'automotive_design',2009,#6008);
#6008=APPLICATION_CONTEXT(
'Core Data for Automotive Mechanical Design Process');
#6009=PRODUCT_CONTEXT('part definition',#6008,'mechanical');
#6010=PRODUCT('Spring-Loaded Scissors','MAS-152','STEP AP214',(#6009));
#6011=PRODUCT('bushing','bushing',$,(#6009));
#6012=PRODUCT('stud','stud',$,(#6009));
#6013=PRODUCT('spring','spring',$,(#6009));
#6014=PRODUCT('Cutting Blade','Cutting Blade',$,(#6009));
#6015=PRODUCT('Forged Aluminum Arm','Forged Aluminum Arm',$,(#6009));
#6016=PRODUCT('Handle Ergonomic Rubber Grip',
'Handle Ergonomic Rubber Grip',$,(#6009));
#6017=PRODUCT('lock','lock',$,(#6009));
#6018=PRESENTATION_STYLE_ASSIGNMENT((#6024));
#6019=PRESENTATION_STYLE_ASSIGNMENT((#6025));
#6020=PRESENTATION_STYLE_ASSIGNMENT((#6026));
#6021=PRESENTATION_STYLE_ASSIGNMENT((#6027));
#6022=PRESENTATION_STYLE_ASSIGNMENT((#6028));
#6023=PRESENTATION_STYLE_ASSIGNMENT((#6029));
#6024=SURFACE_STYLE_USAGE(.BOTH.,#6030);
#6025=SURFACE_STYLE_USAGE(.BOTH.,#6031);
#6026=SURFACE_STYLE_USAGE(.BOTH.,#6032);
#6027=SURFACE_STYLE_USAGE(.BOTH.,#6033);
#6028=SURFACE_STYLE_USAGE(.BOTH.,#6034);
#6029=SURFACE_STYLE_USAGE(.BOTH.,#6035);
#6030=SURFACE_SIDE_STYLE('',(#6036));
#6031=SURFACE_SIDE_STYLE('',(#6037));
#6032=SURFACE_SIDE_STYLE('',(#6038));
#6033=SURFACE_SIDE_STYLE('',(#6039));
#6034=SURFACE_SIDE_STYLE('',(#6040));
#6035=SURFACE_SIDE_STYLE('',(#6041));
#6036=SURFACE_STYLE_FILL_AREA(#6042);
#6037=SURFACE_STYLE_FILL_AREA(#6043);
#6038=SURFACE_STYLE_FILL_AREA(#6044);
#6039=SURFACE_STYLE_FILL_AREA(#6045);
#6040=SURFACE_STYLE_FILL_AREA(#6046);
#6041=SURFACE_STYLE_FILL_AREA(#6047);
#6042=FILL_AREA_STYLE('Steel - Satin',(#6048));
#6043=FILL_AREA_STYLE('Opaque(227,224,212)',(#6049));
#6044=FILL_AREA_STYLE('Opaque(31,36,43)',(#6050));
#6045=FILL_AREA_STYLE('Opaque(122,133,145)',(#6051));
#6046=FILL_AREA_STYLE('Opaque(97,158,199)',(#6052));
#6047=FILL_AREA_STYLE('Opaque(61,176,222)',(#6053));
#6048=FILL_AREA_STYLE_COLOUR('Steel - Satin',#6054);
#6049=FILL_AREA_STYLE_COLOUR('Opaque(227,224,212)',#6055);
#6050=FILL_AREA_STYLE_COLOUR('Opaque(31,36,43)',#6056);
#6051=FILL_AREA_STYLE_COLOUR('Opaque(122,133,145)',#6057);
#6052=FILL_AREA_STYLE_COLOUR('Opaque(97,158,199)',#6058);
#6053=FILL_AREA_STYLE_COLOUR('Opaque(61,176,222)',#6059);
#6054=COLOUR_RGB('Steel - Satin',0.627450980392157,0.627450980392157,0.627450980392157);
#6055=COLOUR_RGB('Opaque(227,224,212)',0.890196078431372,0.87843137254902,
0.831372549019608);
#6056=COLOUR_RGB('Opaque(31,36,43)',0.12156862745098,0.141176470588235,
0.168627450980392);
#6057=COLOUR_RGB('Opaque(122,133,145)',0.47843137254902,0.52156862745098,
0.568627450980392);
#6058=COLOUR_RGB('Opaque(97,158,199)',0.380392156862745,0.619607843137255,
0.780392156862745);
#6059=COLOUR_RGB('Opaque(61,176,222)',0.23921568627451,0.690196078431373,
0.870588235294118);
ENDSEC;
END-ISO-10303-21;
